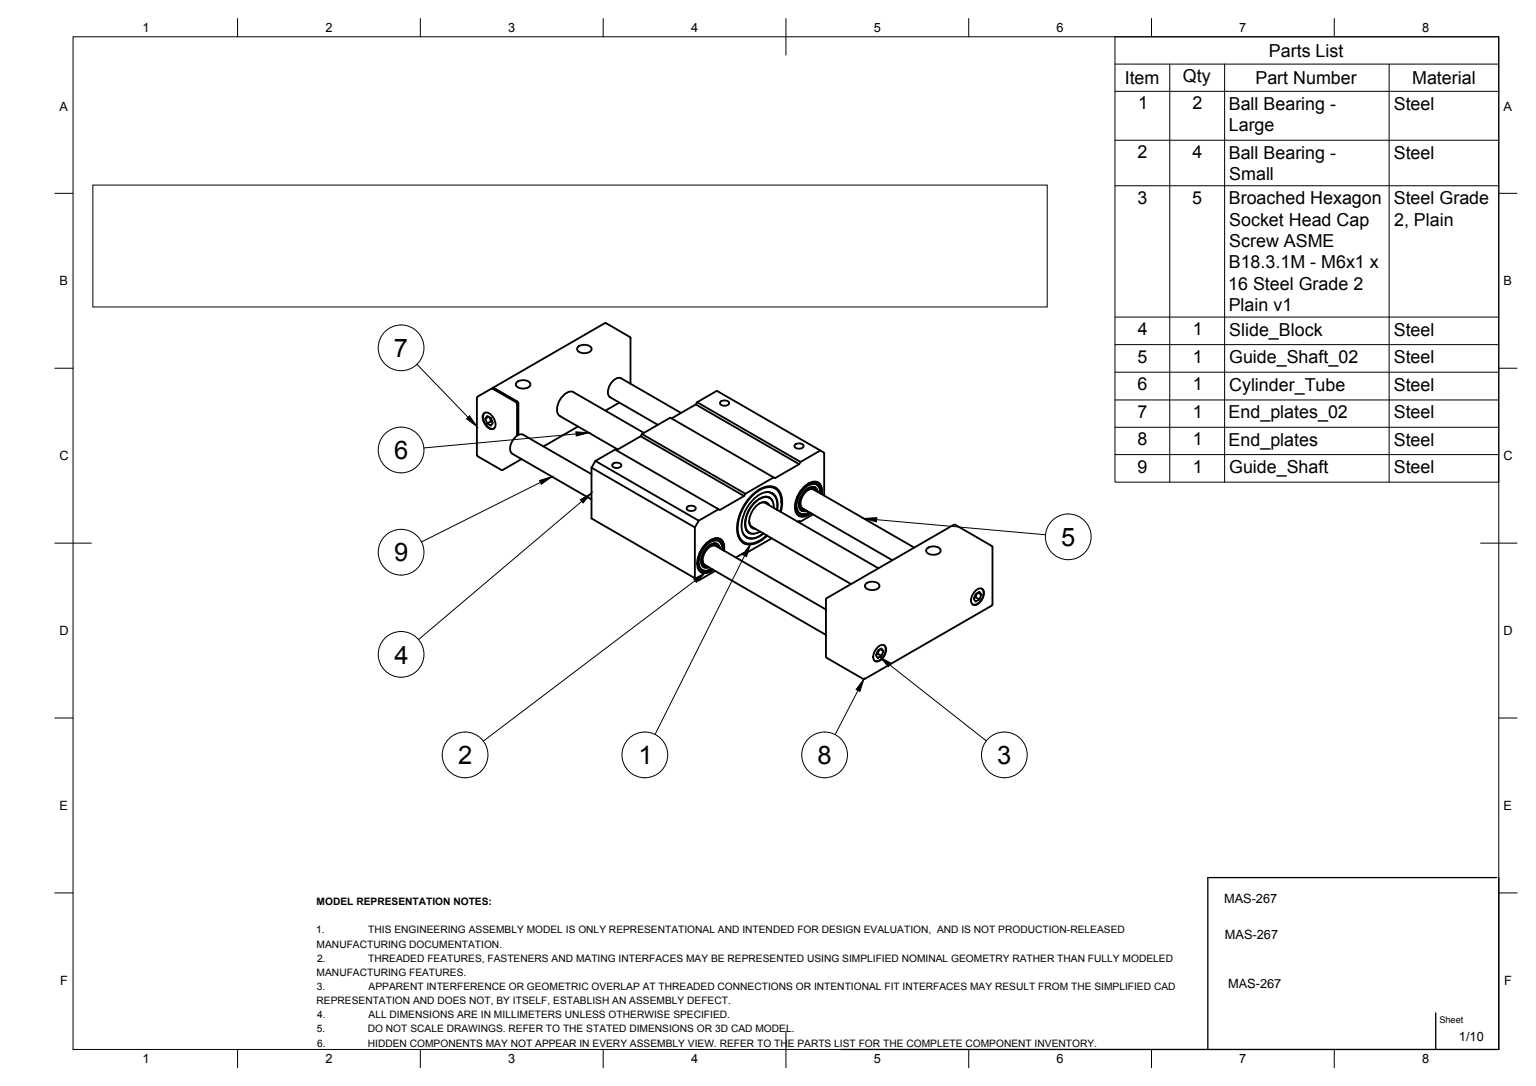
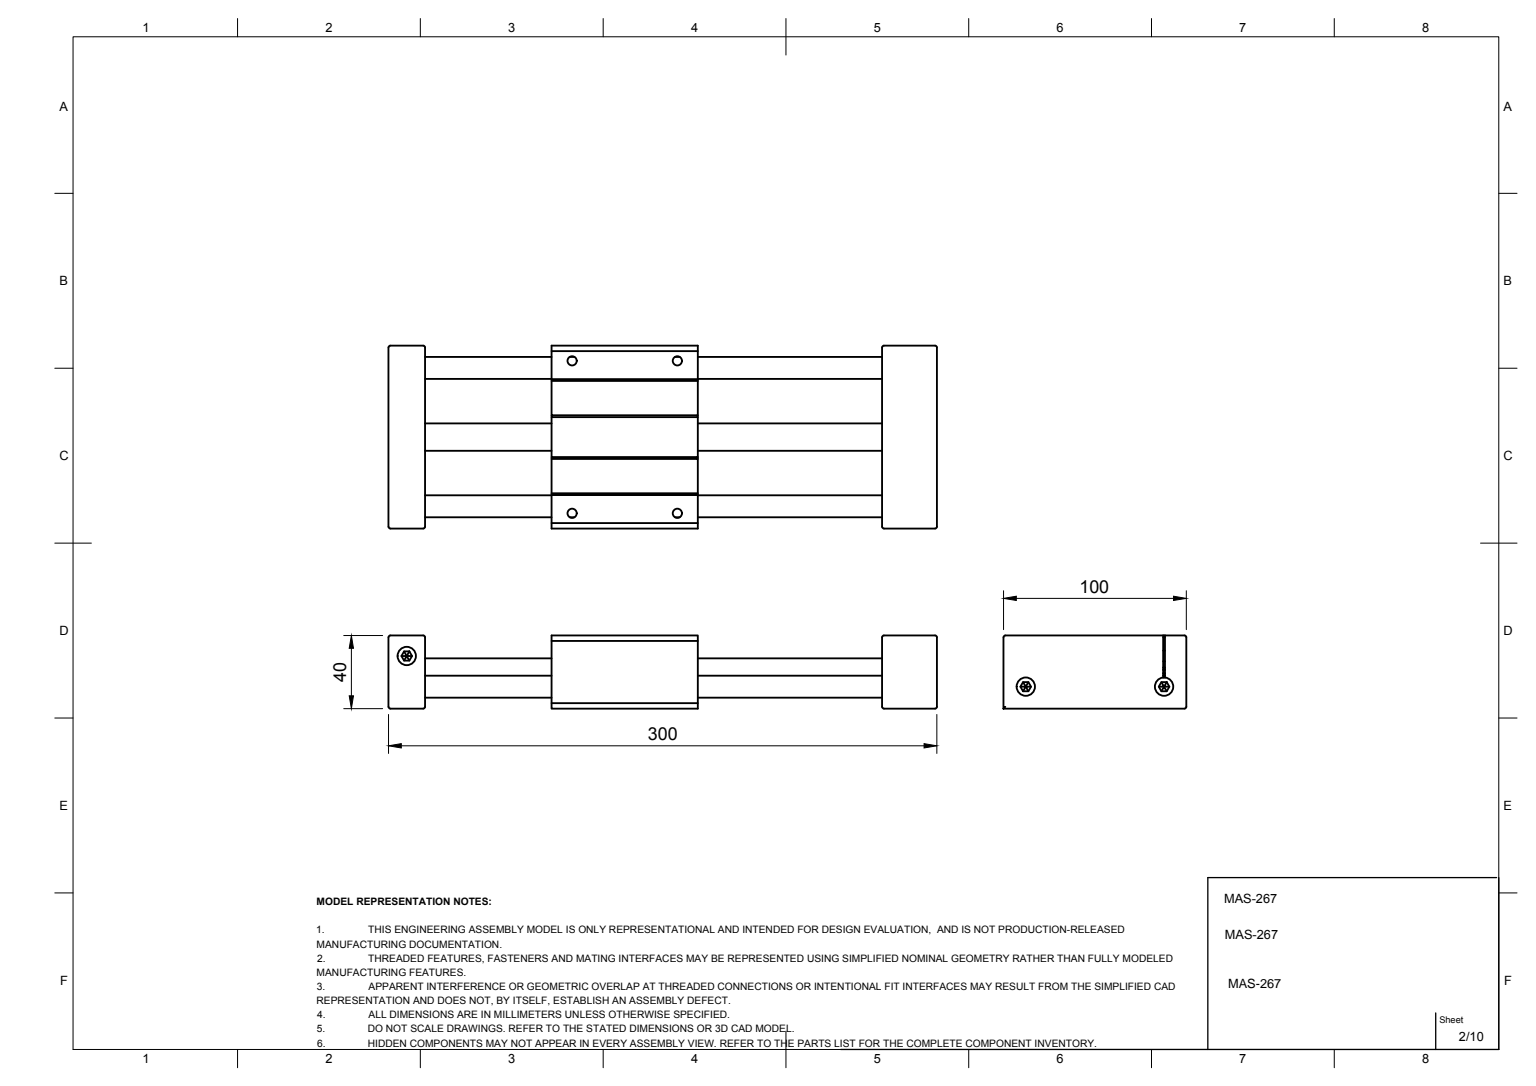
ISO-10303-21;
HEADER;
/* Generated by software containing ST-Developer
 * from STEP Tools, Inc. (www.steptools.com) 
 */

FILE_DESCRIPTION(
/* description */ (''),
/* implementation_level */ '2;1');

FILE_NAME(
/* name */ 'MAS-267',
/* time_stamp */ '2026-10-12T15:29:24-07:00',
/* author */ (''),
/* organization */ (''),
/* preprocessor_version */ 'ST-DEVELOPER v20.2',
/* originating_system */ 'Autodesk Translation Framework v15.15.0.0',
/* authorisation */ '');

FILE_SCHEMA (('AUTOMOTIVE_DESIGN { 1 0 10303 214 3 1 1 }'));
ENDSEC;

DATA;
#10=MECHANICAL_DESIGN_GEOMETRIC_PRESENTATION_REPRESENTATION('',(#163,#164,
#165,#166,#167,#168,#169,#170,#171,#172,#173,#174,#175,#176,#177,#178,#179,
#180,#181,#182,#183,#184,#185,#186,#187,#188,#189,#190,#191,#192,#193,#194,
#195,#196,#197,#198,#199,#200,#201,#202,#203,#204,#205,#206,#207,#208,#209,
#210,#211,#212,#213,#214,#215,#216,#217,#218,#219),#9496);
#11=ITEM_DEFINED_TRANSFORMATION($,$,#5298,#5809);
#12=ITEM_DEFINED_TRANSFORMATION($,$,#5515,#5810);
#13=ITEM_DEFINED_TRANSFORMATION($,$,#5515,#5811);
#14=ITEM_DEFINED_TRANSFORMATION($,$,#5123,#5812);
#15=ITEM_DEFINED_TRANSFORMATION($,$,#5213,#5813);
#16=ITEM_DEFINED_TRANSFORMATION($,$,#5298,#5814);
#17=ITEM_DEFINED_TRANSFORMATION($,$,#5298,#5815);
#18=ITEM_DEFINED_TRANSFORMATION($,$,#5298,#5816);
#19=ITEM_DEFINED_TRANSFORMATION($,$,#5515,#5817);
#20=ITEM_DEFINED_TRANSFORMATION($,$,#5515,#5818);
#21=ITEM_DEFINED_TRANSFORMATION($,$,#5515,#5819);
#22=ITEM_DEFINED_TRANSFORMATION($,$,#5542,#5820);
#23=ITEM_DEFINED_TRANSFORMATION($,$,#5556,#5821);
#24=ITEM_DEFINED_TRANSFORMATION($,$,#5562,#5822);
#25=ITEM_DEFINED_TRANSFORMATION($,$,#5576,#5823);
#26=ITEM_DEFINED_TRANSFORMATION($,$,#5576,#5824);
#27=ITEM_DEFINED_TRANSFORMATION($,$,#5757,#5825);
#28=(
REPRESENTATION_RELATIONSHIP($,$,#9541,#9538)
REPRESENTATION_RELATIONSHIP_WITH_TRANSFORMATION(#11)
SHAPE_REPRESENTATION_RELATIONSHIP()
);
#29=(
REPRESENTATION_RELATIONSHIP($,$,#9542,#9538)
REPRESENTATION_RELATIONSHIP_WITH_TRANSFORMATION(#12)
SHAPE_REPRESENTATION_RELATIONSHIP()
);
#30=(
REPRESENTATION_RELATIONSHIP($,$,#9542,#9538)
REPRESENTATION_RELATIONSHIP_WITH_TRANSFORMATION(#13)
SHAPE_REPRESENTATION_RELATIONSHIP()
);
#31=(
REPRESENTATION_RELATIONSHIP($,$,#9539,#9538)
REPRESENTATION_RELATIONSHIP_WITH_TRANSFORMATION(#14)
SHAPE_REPRESENTATION_RELATIONSHIP()
);
#32=(
REPRESENTATION_RELATIONSHIP($,$,#9540,#9538)
REPRESENTATION_RELATIONSHIP_WITH_TRANSFORMATION(#15)
SHAPE_REPRESENTATION_RELATIONSHIP()
);
#33=(
REPRESENTATION_RELATIONSHIP($,$,#9541,#9538)
REPRESENTATION_RELATIONSHIP_WITH_TRANSFORMATION(#16)
SHAPE_REPRESENTATION_RELATIONSHIP()
);
#34=(
REPRESENTATION_RELATIONSHIP($,$,#9541,#9538)
REPRESENTATION_RELATIONSHIP_WITH_TRANSFORMATION(#17)
SHAPE_REPRESENTATION_RELATIONSHIP()
);
#35=(
REPRESENTATION_RELATIONSHIP($,$,#9541,#9538)
REPRESENTATION_RELATIONSHIP_WITH_TRANSFORMATION(#18)
SHAPE_REPRESENTATION_RELATIONSHIP()
);
#36=(
REPRESENTATION_RELATIONSHIP($,$,#9542,#9538)
REPRESENTATION_RELATIONSHIP_WITH_TRANSFORMATION(#19)
SHAPE_REPRESENTATION_RELATIONSHIP()
);
#37=(
REPRESENTATION_RELATIONSHIP($,$,#9542,#9538)
REPRESENTATION_RELATIONSHIP_WITH_TRANSFORMATION(#20)
SHAPE_REPRESENTATION_RELATIONSHIP()
);
#38=(
REPRESENTATION_RELATIONSHIP($,$,#9542,#9538)
REPRESENTATION_RELATIONSHIP_WITH_TRANSFORMATION(#21)
SHAPE_REPRESENTATION_RELATIONSHIP()
);
#39=(
REPRESENTATION_RELATIONSHIP($,$,#9543,#9538)
REPRESENTATION_RELATIONSHIP_WITH_TRANSFORMATION(#22)
SHAPE_REPRESENTATION_RELATIONSHIP()
);
#40=(
REPRESENTATION_RELATIONSHIP($,$,#9544,#9538)
REPRESENTATION_RELATIONSHIP_WITH_TRANSFORMATION(#23)
SHAPE_REPRESENTATION_RELATIONSHIP()
);
#41=(
REPRESENTATION_RELATIONSHIP($,$,#9545,#9538)
REPRESENTATION_RELATIONSHIP_WITH_TRANSFORMATION(#24)
SHAPE_REPRESENTATION_RELATIONSHIP()
);
#42=(
REPRESENTATION_RELATIONSHIP($,$,#9546,#9538)
REPRESENTATION_RELATIONSHIP_WITH_TRANSFORMATION(#25)
SHAPE_REPRESENTATION_RELATIONSHIP()
);
#43=(
REPRESENTATION_RELATIONSHIP($,$,#9546,#9538)
REPRESENTATION_RELATIONSHIP_WITH_TRANSFORMATION(#26)
SHAPE_REPRESENTATION_RELATIONSHIP()
);
#44=(
REPRESENTATION_RELATIONSHIP($,$,#9547,#9538)
REPRESENTATION_RELATIONSHIP_WITH_TRANSFORMATION(#27)
SHAPE_REPRESENTATION_RELATIONSHIP()
);
#45=CONTEXT_DEPENDENT_SHAPE_REPRESENTATION(#28,#9521);
#46=CONTEXT_DEPENDENT_SHAPE_REPRESENTATION(#29,#9522);
#47=CONTEXT_DEPENDENT_SHAPE_REPRESENTATION(#30,#9523);
#48=CONTEXT_DEPENDENT_SHAPE_REPRESENTATION(#31,#9524);
#49=CONTEXT_DEPENDENT_SHAPE_REPRESENTATION(#32,#9525);
#50=CONTEXT_DEPENDENT_SHAPE_REPRESENTATION(#33,#9526);
#51=CONTEXT_DEPENDENT_SHAPE_REPRESENTATION(#34,#9527);
#52=CONTEXT_DEPENDENT_SHAPE_REPRESENTATION(#35,#9528);
#53=CONTEXT_DEPENDENT_SHAPE_REPRESENTATION(#36,#9529);
#54=CONTEXT_DEPENDENT_SHAPE_REPRESENTATION(#37,#9530);
#55=CONTEXT_DEPENDENT_SHAPE_REPRESENTATION(#38,#9531);
#56=CONTEXT_DEPENDENT_SHAPE_REPRESENTATION(#39,#9532);
#57=CONTEXT_DEPENDENT_SHAPE_REPRESENTATION(#40,#9533);
#58=CONTEXT_DEPENDENT_SHAPE_REPRESENTATION(#41,#9534);
#59=CONTEXT_DEPENDENT_SHAPE_REPRESENTATION(#42,#9535);
#60=CONTEXT_DEPENDENT_SHAPE_REPRESENTATION(#43,#9536);
#61=CONTEXT_DEPENDENT_SHAPE_REPRESENTATION(#44,#9537);
#62=NEXT_ASSEMBLY_USAGE_OCCURRENCE('Ball Bearing - Small:1',
'Ball Bearing - Small:1','Ball Bearing - Small:1',#9549,#9552,
'Ball Bearing - Small:1');
#63=NEXT_ASSEMBLY_USAGE_OCCURRENCE(
'Broached Hexagon Socket Head Cap Screw ASME B18.3.1M - M6x1 x 16 Stee
l Grade 2 Plain v1:1',
'Broached Hexagon Socket Head Cap Screw ASME B18.3.1M - M6x1 x 16 Stee
l Grade 2 Plain v1:1',
'Broached Hexagon Socket Head Cap Screw ASME B18.3.1M - M6x1 x 16 Stee
l Grade 2 Plain v1:1',#9549,#9553,
'Broached Hexagon Socket Head Cap Screw ASME B18.3.1M - M6x1 x 16 Stee
l Grade 2 Plain v1:1');
#64=NEXT_ASSEMBLY_USAGE_OCCURRENCE(
'Broached Hexagon Socket Head Cap Screw ASME B18.3.1M - M6x1 x 16 Stee
l Grade 2 Plain v1:2',
'Broached Hexagon Socket Head Cap Screw ASME B18.3.1M - M6x1 x 16 Stee
l Grade 2 Plain v1:2',
'Broached Hexagon Socket Head Cap Screw ASME B18.3.1M - M6x1 x 16 Stee
l Grade 2 Plain v1:2',#9549,#9553,
'Broached Hexagon Socket Head Cap Screw ASME B18.3.1M - M6x1 x 16 Stee
l Grade 2 Plain v1:2');
#65=NEXT_ASSEMBLY_USAGE_OCCURRENCE('End_plates_02:1','End_plates_02:1',
'End_plates_02:1',#9549,#9550,'End_plates_02:1');
#66=NEXT_ASSEMBLY_USAGE_OCCURRENCE('End_plates:1','End_plates:1',
'End_plates:1',#9549,#9551,'End_plates:1');
#67=NEXT_ASSEMBLY_USAGE_OCCURRENCE('Ball Bearing - Small:2',
'Ball Bearing - Small:2','Ball Bearing - Small:2',#9549,#9552,
'Ball Bearing - Small:2');
#68=NEXT_ASSEMBLY_USAGE_OCCURRENCE('Ball Bearing - Small:3',
'Ball Bearing - Small:3','Ball Bearing - Small:3',#9549,#9552,
'Ball Bearing - Small:3');
#69=NEXT_ASSEMBLY_USAGE_OCCURRENCE('Ball Bearing - Small:4',
'Ball Bearing - Small:4','Ball Bearing - Small:4',#9549,#9552,
'Ball Bearing - Small:4');
#70=NEXT_ASSEMBLY_USAGE_OCCURRENCE(
'Broached Hexagon Socket Head Cap Screw ASME B18.3.1M - M6x1 x 16 Stee
l Grade 2 Plain v1:3',
'Broached Hexagon Socket Head Cap Screw ASME B18.3.1M - M6x1 x 16 Stee
l Grade 2 Plain v1:3',
'Broached Hexagon Socket Head Cap Screw ASME B18.3.1M - M6x1 x 16 Stee
l Grade 2 Plain v1:3',#9549,#9553,
'Broached Hexagon Socket Head Cap Screw ASME B18.3.1M - M6x1 x 16 Stee
l Grade 2 Plain v1:3');
#71=NEXT_ASSEMBLY_USAGE_OCCURRENCE(
'Broached Hexagon Socket Head Cap Screw ASME B18.3.1M - M6x1 x 16 Stee
l Grade 2 Plain v1:4',
'Broached Hexagon Socket Head Cap Screw ASME B18.3.1M - M6x1 x 16 Stee
l Grade 2 Plain v1:4',
'Broached Hexagon Socket Head Cap Screw ASME B18.3.1M - M6x1 x 16 Stee
l Grade 2 Plain v1:4',#9549,#9553,
'Broached Hexagon Socket Head Cap Screw ASME B18.3.1M - M6x1 x 16 Stee
l Grade 2 Plain v1:4');
#72=NEXT_ASSEMBLY_USAGE_OCCURRENCE(
'Broached Hexagon Socket Head Cap Screw ASME B18.3.1M - M6x1 x 16 Stee
l Grade 2 Plain v1:5',
'Broached Hexagon Socket Head Cap Screw ASME B18.3.1M - M6x1 x 16 Stee
l Grade 2 Plain v1:5',
'Broached Hexagon Socket Head Cap Screw ASME B18.3.1M - M6x1 x 16 Stee
l Grade 2 Plain v1:5',#9549,#9553,
'Broached Hexagon Socket Head Cap Screw ASME B18.3.1M - M6x1 x 16 Stee
l Grade 2 Plain v1:5');
#73=NEXT_ASSEMBLY_USAGE_OCCURRENCE('Guide_Shaft_02:1',
'Guide_Shaft_02:1','Guide_Shaft_02:1',#9549,#9554,'Guide_Shaft_02:1');
#74=NEXT_ASSEMBLY_USAGE_OCCURRENCE('Cylinder_Tube:1','Cylinder_Tube:1',
'Cylinder_Tube:1',#9549,#9555,'Cylinder_Tube:1');
#75=NEXT_ASSEMBLY_USAGE_OCCURRENCE('Guide_Shaft:1','Guide_Shaft:1',
'Guide_Shaft:1',#9549,#9556,'Guide_Shaft:1');
#76=NEXT_ASSEMBLY_USAGE_OCCURRENCE('Ball Bearing - Large:1',
'Ball Bearing - Large:1','Ball Bearing - Large:1',#9549,#9557,
'Ball Bearing - Large:1');
#77=NEXT_ASSEMBLY_USAGE_OCCURRENCE('Ball Bearing - Large:2',
'Ball Bearing - Large:2','Ball Bearing - Large:2',#9549,#9557,
'Ball Bearing - Large:2');
#78=NEXT_ASSEMBLY_USAGE_OCCURRENCE('Slide_Block:1','Slide_Block:1',
'Slide_Block:1',#9549,#9558,'Slide_Block:1');
#79=B_SPLINE_CURVE_WITH_KNOTS('',3,(#8964,#8965,#8966,#8967,#8968,#8969,
#8970,#8971,#8972,#8973),.UNSPECIFIED.,.F.,.F.,(4,2,2,2,4),(-1.57648415340294,
-1.48130138260372,-1.38611861180451,-1.27940954804234,-1.17270048428017),
 .UNSPECIFIED.);
#80=B_SPLINE_CURVE_WITH_KNOTS('',3,(#8974,#8975,#8976,#8977,#8978,#8979,
#8980,#8981,#8982,#8983,#8984,#8985,#8986,#8987,#8988,#8989,#8990,#8991,
#8992,#8993,#8994,#8995,#8996,#8997,#8998,#8999),.UNSPECIFIED.,.F.,.F.,
(4,2,2,2,2,2,2,2,2,2,2,2,4),(-1.17270048428017,-1.07435447096729,-0.976008457654416,
-0.882125267177943,-0.78824207670147,-0.694358886224997,-0.600475695748524,
-0.502129682435648,-0.403783669122773,-0.297074605360601,-0.190365541598429,
-0.0951827707992146,0.),.UNSPECIFIED.);
#81=B_SPLINE_CURVE_WITH_KNOTS('',3,(#9003,#9004,#9005,#9006,#9007,#9008,
#9009,#9010,#9011,#9012,#9013,#9014,#9015,#9016,#9017,#9018,#9019,#9020,
#9021,#9022,#9023,#9024,#9025,#9026,#9027,#9028),.UNSPECIFIED.,.F.,.F.,
(4,2,2,2,2,2,2,2,2,2,2,2,4),(-1.57648415340294,-1.48130138260372,-1.38611861180451,
-1.27940954804234,-1.17270048428017,-1.07435447096729,-0.976008457654416,
-0.882125267177943,-0.78824207670147,-0.694358886224997,-0.600475695748524,
-0.502129682435648,-0.403783669122773),.UNSPECIFIED.);
#82=B_SPLINE_CURVE_WITH_KNOTS('',3,(#9029,#9030,#9031,#9032,#9033,#9034,
#9035,#9036,#9037,#9038),.UNSPECIFIED.,.F.,.F.,(4,2,2,2,4),(-0.403783669122773,
-0.297074605360601,-0.190365541598429,-0.0951827707992147,0.),
 .UNSPECIFIED.);
#83=B_SPLINE_CURVE_WITH_KNOTS('',3,(#9048,#9049,#9050,#9051,#9052,#9053,
#9054,#9055,#9056,#9057,#9058,#9059,#9060,#9061,#9062,#9063,#9064,#9065,
#9066,#9067,#9068,#9069,#9070,#9071,#9072,#9073),.UNSPECIFIED.,.F.,.F.,
(4,2,2,2,2,2,2,2,2,2,2,2,4),(-1.57648415340294,-1.48130138260372,-1.38611861180451,
-1.27940954804234,-1.17270048428017,-1.07435447096729,-0.976008457654416,
-0.882125267177943,-0.78824207670147,-0.694358886224997,-0.600475695748524,
-0.502129682435648,-0.403783669122773),.UNSPECIFIED.);
#84=B_SPLINE_CURVE_WITH_KNOTS('',3,(#9074,#9075,#9076,#9077,#9078,#9079,
#9080,#9081,#9082,#9083),.UNSPECIFIED.,.F.,.F.,(4,2,2,2,4),(-0.403783669122773,
-0.297074605360601,-0.190365541598429,-0.0951827707992146,0.),
 .UNSPECIFIED.);
#85=B_SPLINE_CURVE_WITH_KNOTS('',3,(#9087,#9088,#9089,#9090,#9091,#9092,
#9093,#9094,#9095,#9096),.UNSPECIFIED.,.F.,.F.,(4,2,2,2,4),(-1.57648415340294,
-1.48130138260372,-1.38611861180451,-1.27940954804234,-1.17270048428017),
 .UNSPECIFIED.);
#86=B_SPLINE_CURVE_WITH_KNOTS('',3,(#9097,#9098,#9099,#9100,#9101,#9102,
#9103,#9104,#9105,#9106,#9107,#9108,#9109,#9110,#9111,#9112,#9113,#9114,
#9115,#9116,#9117,#9118,#9119,#9120,#9121,#9122),.UNSPECIFIED.,.F.,.F.,
(4,2,2,2,2,2,2,2,2,2,2,2,4),(-1.17270048428017,-1.07435447096729,-0.976008457654416,
-0.882125267177943,-0.78824207670147,-0.694358886224997,-0.600475695748524,
-0.502129682435648,-0.403783669122773,-0.297074605360601,-0.190365541598429,
-0.0951827707992147,0.),.UNSPECIFIED.);
#87=B_SPLINE_CURVE_WITH_KNOTS('',3,(#9132,#9133,#9134,#9135,#9136,#9137,
#9138,#9139,#9140,#9141),.UNSPECIFIED.,.F.,.F.,(4,2,2,2,4),(-1.57648415340294,
-1.48130138260372,-1.38611861180451,-1.27940954804234,-1.17270048428017),
 .UNSPECIFIED.);
#88=B_SPLINE_CURVE_WITH_KNOTS('',3,(#9142,#9143,#9144,#9145,#9146,#9147,
#9148,#9149,#9150,#9151,#9152,#9153,#9154,#9155,#9156,#9157,#9158,#9159,
#9160,#9161,#9162,#9163,#9164,#9165,#9166,#9167),.UNSPECIFIED.,.F.,.F.,
(4,2,2,2,2,2,2,2,2,2,2,2,4),(-1.17270048428017,-1.07435447096729,-0.976008457654416,
-0.882125267177943,-0.78824207670147,-0.694358886224997,-0.600475695748524,
-0.502129682435648,-0.403783669122773,-0.297074605360601,-0.190365541598429,
-0.0951827707992146,0.),.UNSPECIFIED.);
#89=B_SPLINE_CURVE_WITH_KNOTS('',3,(#9171,#9172,#9173,#9174,#9175,#9176,
#9177,#9178,#9179,#9180,#9181,#9182,#9183,#9184,#9185,#9186,#9187,#9188,
#9189,#9190,#9191,#9192,#9193,#9194,#9195,#9196),.UNSPECIFIED.,.F.,.F.,
(4,2,2,2,2,2,2,2,2,2,2,2,4),(-1.57648415340294,-1.48130138260372,-1.38611861180451,
-1.27940954804234,-1.17270048428017,-1.07435447096729,-0.976008457654416,
-0.882125267177943,-0.78824207670147,-0.694358886224997,-0.600475695748524,
-0.502129682435648,-0.403783669122773),.UNSPECIFIED.);
#90=B_SPLINE_CURVE_WITH_KNOTS('',3,(#9197,#9198,#9199,#9200,#9201,#9202,
#9203,#9204,#9205,#9206),.UNSPECIFIED.,.F.,.F.,(4,2,2,2,4),(-0.403783669122773,
-0.297074605360601,-0.190365541598429,-0.0951827707992147,0.),
 .UNSPECIFIED.);
#91=B_SPLINE_CURVE_WITH_KNOTS('',3,(#9216,#9217,#9218,#9219,#9220,#9221,
#9222,#9223,#9224,#9225,#9226,#9227,#9228,#9229,#9230,#9231,#9232,#9233,
#9234,#9235,#9236,#9237,#9238,#9239,#9240,#9241),.UNSPECIFIED.,.F.,.F.,
(4,2,2,2,2,2,2,2,2,2,2,2,4),(-1.57648415340294,-1.48130138260372,-1.38611861180451,
-1.27940954804234,-1.17270048428017,-1.07435447096729,-0.976008457654416,
-0.882125267177943,-0.78824207670147,-0.694358886224997,-0.600475695748524,
-0.502129682435648,-0.403783669122773),.UNSPECIFIED.);
#92=B_SPLINE_CURVE_WITH_KNOTS('',3,(#9242,#9243,#9244,#9245,#9246,#9247,
#9248,#9249,#9250,#9251),.UNSPECIFIED.,.F.,.F.,(4,2,2,2,4),(-0.403783669122773,
-0.297074605360601,-0.190365541598429,-0.0951827707992146,0.),
 .UNSPECIFIED.);
#93=B_SPLINE_CURVE_WITH_KNOTS('',3,(#9255,#9256,#9257,#9258,#9259,#9260,
#9261,#9262,#9263,#9264),.UNSPECIFIED.,.F.,.F.,(4,2,2,2,4),(-1.57648415340294,
-1.48130138260372,-1.38611861180451,-1.27940954804234,-1.17270048428017),
 .UNSPECIFIED.);
#94=B_SPLINE_CURVE_WITH_KNOTS('',3,(#9265,#9266,#9267,#9268,#9269,#9270,
#9271,#9272,#9273,#9274,#9275,#9276,#9277,#9278,#9279,#9280,#9281,#9282,
#9283,#9284,#9285,#9286,#9287,#9288,#9289,#9290),.UNSPECIFIED.,.F.,.F.,
(4,2,2,2,2,2,2,2,2,2,2,2,4),(-1.17270048428017,-1.07435447096729,-0.976008457654416,
-0.882125267177943,-0.78824207670147,-0.694358886224997,-0.600475695748524,
-0.502129682435648,-0.403783669122773,-0.297074605360601,-0.190365541598429,
-0.0951827707992147,0.),.UNSPECIFIED.);
#95=(
BOUNDED_SURFACE()
B_SPLINE_SURFACE(2,2,((#7928,#7929,#7930,#7931,#7932,#7933,#7934,#7935,
#7936),(#7937,#7938,#7939,#7940,#7941,#7942,#7943,#7944,#7945),(#7946,#7947,
#7948,#7949,#7950,#7951,#7952,#7953,#7954)),.UNSPECIFIED.,.F.,.T.,.F.)
B_SPLINE_SURFACE_WITH_KNOTS((3,3),(3,2,2,2,3),(-0.359817990374321,0.359817990374321),
(-3.14159265358979,-1.5707963267949,0.,1.5707963267949,3.14159265358979),
 .UNSPECIFIED.)
GEOMETRIC_REPRESENTATION_ITEM()
RATIONAL_B_SPLINE_SURFACE(((1.,0.707106781186548,1.,0.707106781186548,1.,
0.707106781186548,1.,0.707106781186548,1.),(0.935960925476955,0.661824317330392,
0.935960925476955,0.661824317330392,0.935960925476955,0.661824317330392,
0.935960925476955,0.661824317330392,0.935960925476955),(1.,0.707106781186548,
1.,0.707106781186548,1.,0.707106781186548,1.,0.707106781186548,1.)))
REPRESENTATION_ITEM('')
SURFACE()
);
#96=(
BOUNDED_SURFACE()
B_SPLINE_SURFACE(2,2,((#7970,#7971,#7972,#7973,#7974,#7975,#7976,#7977,
#7978),(#7979,#7980,#7981,#7982,#7983,#7984,#7985,#7986,#7987),(#7988,#7989,
#7990,#7991,#7992,#7993,#7994,#7995,#7996)),.UNSPECIFIED.,.F.,.T.,.F.)
B_SPLINE_SURFACE_WITH_KNOTS((3,3),(3,2,2,2,3),(-0.359817990374415,0.359817990374426),
(-3.14159265358979,-1.5707963267949,0.,1.5707963267949,3.14159265358979),
 .UNSPECIFIED.)
GEOMETRIC_REPRESENTATION_ITEM()
RATIONAL_B_SPLINE_SURFACE(((1.,0.707106781186548,1.,0.707106781186548,1.,
0.707106781186548,1.,0.707106781186548,1.),(0.935960925476919,0.661824317330366,
0.935960925476919,0.661824317330366,0.935960925476919,0.661824317330366,
0.935960925476919,0.661824317330366,0.935960925476919),(1.,0.707106781186548,
1.,0.707106781186548,1.,0.707106781186548,1.,0.707106781186548,1.)))
REPRESENTATION_ITEM('')
SURFACE()
);
#97=(
BOUNDED_SURFACE()
B_SPLINE_SURFACE(2,2,((#8012,#8013,#8014,#8015,#8016,#8017,#8018,#8019,
#8020),(#8021,#8022,#8023,#8024,#8025,#8026,#8027,#8028,#8029),(#8030,#8031,
#8032,#8033,#8034,#8035,#8036,#8037,#8038)),.UNSPECIFIED.,.F.,.T.,.F.)
B_SPLINE_SURFACE_WITH_KNOTS((3,3),(3,2,2,2,3),(-0.359817990374342,0.359817990374333),
(-3.14159265358979,-1.5707963267949,0.,1.5707963267949,3.14159265358979),
 .UNSPECIFIED.)
GEOMETRIC_REPRESENTATION_ITEM()
RATIONAL_B_SPLINE_SURFACE(((1.,0.707106781186548,1.,0.707106781186548,1.,
0.707106781186548,1.,0.707106781186548,1.),(0.935960925476941,0.661824317330382,
0.935960925476941,0.661824317330382,0.935960925476941,0.661824317330382,
0.935960925476941,0.661824317330382,0.935960925476941),(1.,0.707106781186548,
1.,0.707106781186548,1.,0.707106781186548,1.,0.707106781186548,1.)))
REPRESENTATION_ITEM('')
SURFACE()
);
#98=(
BOUNDED_SURFACE()
B_SPLINE_SURFACE(2,2,((#8054,#8055,#8056,#8057,#8058,#8059,#8060,#8061,
#8062),(#8063,#8064,#8065,#8066,#8067,#8068,#8069,#8070,#8071),(#8072,#8073,
#8074,#8075,#8076,#8077,#8078,#8079,#8080)),.UNSPECIFIED.,.F.,.T.,.F.)
B_SPLINE_SURFACE_WITH_KNOTS((3,3),(3,2,2,2,3),(-0.359817990374327,0.359817990374343),
(-3.14159265358979,-1.5707963267949,0.,1.5707963267949,3.14159265358979),
 .UNSPECIFIED.)
GEOMETRIC_REPRESENTATION_ITEM()
RATIONAL_B_SPLINE_SURFACE(((1.,0.707106781186548,1.,0.707106781186548,1.,
0.707106781186548,1.,0.707106781186548,1.),(0.935960925476945,0.661824317330385,
0.935960925476945,0.661824317330385,0.935960925476945,0.661824317330385,
0.935960925476945,0.661824317330385,0.935960925476945),(1.,0.707106781186548,
1.,0.707106781186548,1.,0.707106781186548,1.,0.707106781186548,1.)))
REPRESENTATION_ITEM('')
SURFACE()
);
#99=(
BOUNDED_SURFACE()
B_SPLINE_SURFACE(2,2,((#8096,#8097,#8098,#8099,#8100,#8101,#8102,#8103,
#8104),(#8105,#8106,#8107,#8108,#8109,#8110,#8111,#8112,#8113),(#8114,#8115,
#8116,#8117,#8118,#8119,#8120,#8121,#8122)),.UNSPECIFIED.,.F.,.T.,.F.)
B_SPLINE_SURFACE_WITH_KNOTS((3,3),(3,2,2,2,3),(-0.359817990374369,0.359817990374379),
(-3.14159265358979,-1.5707963267949,0.,1.5707963267949,3.14159265358979),
 .UNSPECIFIED.)
GEOMETRIC_REPRESENTATION_ITEM()
RATIONAL_B_SPLINE_SURFACE(((1.,0.707106781186548,1.,0.707106781186548,1.,
0.707106781186548,1.,0.707106781186548,1.),(0.935960925476939,0.661824317330381,
0.935960925476939,0.661824317330381,0.935960925476939,0.661824317330381,
0.935960925476939,0.661824317330381,0.935960925476939),(1.,0.707106781186548,
1.,0.707106781186548,1.,0.707106781186548,1.,0.707106781186548,1.)))
REPRESENTATION_ITEM('')
SURFACE()
);
#100=(
BOUNDED_SURFACE()
B_SPLINE_SURFACE(2,2,((#8138,#8139,#8140,#8141,#8142,#8143,#8144,#8145,
#8146),(#8147,#8148,#8149,#8150,#8151,#8152,#8153,#8154,#8155),(#8156,#8157,
#8158,#8159,#8160,#8161,#8162,#8163,#8164)),.UNSPECIFIED.,.F.,.T.,.F.)
B_SPLINE_SURFACE_WITH_KNOTS((3,3),(3,2,2,2,3),(-0.359817990374391,0.359817990374391),
(-3.14159265358979,-1.5707963267949,0.,1.5707963267949,3.14159265358979),
 .UNSPECIFIED.)
GEOMETRIC_REPRESENTATION_ITEM()
RATIONAL_B_SPLINE_SURFACE(((1.,0.707106781186548,1.,0.707106781186548,1.,
0.707106781186548,1.,0.707106781186548,1.),(0.935960925476929,0.661824317330373,
0.935960925476929,0.661824317330373,0.935960925476929,0.661824317330373,
0.935960925476929,0.661824317330373,0.935960925476929),(1.,0.707106781186548,
1.,0.707106781186548,1.,0.707106781186548,1.,0.707106781186548,1.)))
REPRESENTATION_ITEM('')
SURFACE()
);
#101=(
BOUNDED_SURFACE()
B_SPLINE_SURFACE(2,2,((#8180,#8181,#8182,#8183,#8184,#8185,#8186,#8187,
#8188),(#8189,#8190,#8191,#8192,#8193,#8194,#8195,#8196,#8197),(#8198,#8199,
#8200,#8201,#8202,#8203,#8204,#8205,#8206)),.UNSPECIFIED.,.F.,.T.,.F.)
B_SPLINE_SURFACE_WITH_KNOTS((3,3),(3,2,2,2,3),(-0.359817990374328,0.359817990374325),
(-3.14159265358979,-1.5707963267949,0.,1.5707963267949,3.14159265358979),
 .UNSPECIFIED.)
GEOMETRIC_REPRESENTATION_ITEM()
RATIONAL_B_SPLINE_SURFACE(((1.,0.707106781186548,1.,0.707106781186548,1.,
0.707106781186548,1.,0.707106781186548,1.),(0.935960925476951,0.661824317330389,
0.935960925476951,0.661824317330389,0.935960925476951,0.661824317330389,
0.935960925476951,0.661824317330389,0.935960925476951),(1.,0.707106781186548,
1.,0.707106781186548,1.,0.707106781186548,1.,0.707106781186548,1.)))
REPRESENTATION_ITEM('')
SURFACE()
);
#102=(
BOUNDED_SURFACE()
B_SPLINE_SURFACE(2,2,((#8222,#8223,#8224,#8225,#8226,#8227,#8228,#8229,
#8230),(#8231,#8232,#8233,#8234,#8235,#8236,#8237,#8238,#8239),(#8240,#8241,
#8242,#8243,#8244,#8245,#8246,#8247,#8248)),.UNSPECIFIED.,.F.,.T.,.F.)
B_SPLINE_SURFACE_WITH_KNOTS((3,3),(3,2,2,2,3),(-0.359817990374346,0.359817990374343),
(-3.14159265358979,-1.5707963267949,0.,1.5707963267949,3.14159265358979),
 .UNSPECIFIED.)
GEOMETRIC_REPRESENTATION_ITEM()
RATIONAL_B_SPLINE_SURFACE(((1.,0.707106781186548,1.,0.707106781186548,1.,
0.707106781186548,1.,0.707106781186548,1.),(0.935960925476942,0.661824317330383,
0.935960925476942,0.661824317330383,0.935960925476942,0.661824317330383,
0.935960925476942,0.661824317330383,0.935960925476942),(1.,0.707106781186548,
1.,0.707106781186548,1.,0.707106781186548,1.,0.707106781186548,1.)))
REPRESENTATION_ITEM('')
SURFACE()
);
#103=(
BOUNDED_SURFACE()
B_SPLINE_SURFACE(2,2,((#8264,#8265,#8266,#8267,#8268,#8269,#8270,#8271,
#8272),(#8273,#8274,#8275,#8276,#8277,#8278,#8279,#8280,#8281),(#8282,#8283,
#8284,#8285,#8286,#8287,#8288,#8289,#8290)),.UNSPECIFIED.,.F.,.T.,.F.)
B_SPLINE_SURFACE_WITH_KNOTS((3,3),(3,2,2,2,3),(-0.359817990374353,0.359817990374347),
(-3.14159265358979,-1.5707963267949,0.,1.5707963267949,3.14159265358979),
 .UNSPECIFIED.)
GEOMETRIC_REPRESENTATION_ITEM()
RATIONAL_B_SPLINE_SURFACE(((1.,0.707106781186548,1.,0.707106781186548,1.,
0.707106781186548,1.,0.707106781186548,1.),(0.935960925476944,0.661824317330384,
0.935960925476944,0.661824317330384,0.935960925476944,0.661824317330384,
0.935960925476944,0.661824317330384,0.935960925476944),(1.,0.707106781186548,
1.,0.707106781186548,1.,0.707106781186548,1.,0.707106781186548,1.)))
REPRESENTATION_ITEM('')
SURFACE()
);
#104=(
BOUNDED_SURFACE()
B_SPLINE_SURFACE(2,2,((#8306,#8307,#8308,#8309,#8310,#8311,#8312,#8313,
#8314),(#8315,#8316,#8317,#8318,#8319,#8320,#8321,#8322,#8323),(#8324,#8325,
#8326,#8327,#8328,#8329,#8330,#8331,#8332)),.UNSPECIFIED.,.F.,.T.,.F.)
B_SPLINE_SURFACE_WITH_KNOTS((3,3),(3,2,2,2,3),(-0.359817990374389,0.359817990374389),
(-3.14159265358979,-1.5707963267949,0.,1.5707963267949,3.14159265358979),
 .UNSPECIFIED.)
GEOMETRIC_REPRESENTATION_ITEM()
RATIONAL_B_SPLINE_SURFACE(((1.,0.707106781186548,1.,0.707106781186548,1.,
0.707106781186548,1.,0.707106781186548,1.),(0.935960925476925,0.661824317330371,
0.935960925476925,0.661824317330371,0.935960925476925,0.661824317330371,
0.935960925476925,0.661824317330371,0.935960925476925),(1.,0.707106781186548,
1.,0.707106781186548,1.,0.707106781186548,1.,0.707106781186548,1.)))
REPRESENTATION_ITEM('')
SURFACE()
);
#105=(
BOUNDED_SURFACE()
B_SPLINE_SURFACE(2,2,((#8362,#8363,#8364,#8365,#8366,#8367,#8368,#8369,
#8370),(#8371,#8372,#8373,#8374,#8375,#8376,#8377,#8378,#8379),(#8380,#8381,
#8382,#8383,#8384,#8385,#8386,#8387,#8388)),.UNSPECIFIED.,.F.,.T.,.F.)
B_SPLINE_SURFACE_WITH_KNOTS((3,3),(3,2,2,2,3),(-0.359817990374337,0.359817990374338),
(-3.14159265358979,-1.5707963267949,0.,1.5707963267949,3.14159265358979),
 .UNSPECIFIED.)
GEOMETRIC_REPRESENTATION_ITEM()
RATIONAL_B_SPLINE_SURFACE(((1.,0.707106781186548,1.,0.707106781186548,1.,
0.707106781186548,1.,0.707106781186548,1.),(0.935960925476947,0.661824317330386,
0.935960925476947,0.661824317330386,0.935960925476947,0.661824317330386,
0.935960925476947,0.661824317330386,0.935960925476947),(1.,0.707106781186548,
1.,0.707106781186548,1.,0.707106781186548,1.,0.707106781186548,1.)))
REPRESENTATION_ITEM('')
SURFACE()
);
#106=(
BOUNDED_SURFACE()
B_SPLINE_SURFACE(2,2,((#8404,#8405,#8406,#8407,#8408,#8409,#8410,#8411,
#8412),(#8413,#8414,#8415,#8416,#8417,#8418,#8419,#8420,#8421),(#8422,#8423,
#8424,#8425,#8426,#8427,#8428,#8429,#8430)),.UNSPECIFIED.,.F.,.T.,.F.)
B_SPLINE_SURFACE_WITH_KNOTS((3,3),(3,2,2,2,3),(-0.359817990374313,0.359817990374317),
(-3.14159265358979,-1.5707963267949,0.,1.5707963267949,3.14159265358979),
 .UNSPECIFIED.)
GEOMETRIC_REPRESENTATION_ITEM()
RATIONAL_B_SPLINE_SURFACE(((1.,0.707106781186548,1.,0.707106781186548,1.,
0.707106781186548,1.,0.707106781186548,1.),(0.935960925476952,0.66182431733039,
0.935960925476952,0.66182431733039,0.935960925476952,0.66182431733039,0.935960925476952,
0.66182431733039,0.935960925476952),(1.,0.707106781186548,1.,0.707106781186548,
1.,0.707106781186548,1.,0.707106781186548,1.)))
REPRESENTATION_ITEM('')
SURFACE()
);
#107=CONICAL_SURFACE('',#5303,6.24999999999999,0.785398163397428);
#108=CONICAL_SURFACE('',#5309,6.,0.785398163397428);
#109=CONICAL_SURFACE('',#5319,10.25,0.785398163397433);
#110=CONICAL_SURFACE('',#5330,10.5,0.785398163397433);
#111=CONICAL_SURFACE('',#5488,9.25000000000001,1.01776488264426);
#112=CONICAL_SURFACE('',#5490,7.39999999999999,1.01776488264426);
#113=CONICAL_SURFACE('',#5507,7.24999999999999,1.01776488264426);
#114=CONICAL_SURFACE('',#5509,9.1,1.01776488264426);
#115=CONICAL_SURFACE('',#5516,2.72327499999996,0.831988093682975);
#116=CONICAL_SURFACE('',#5581,8.04999999999999,0.78539816339744);
#117=CONICAL_SURFACE('',#5587,7.5,0.78539816339744);
#118=CONICAL_SURFACE('',#5597,16.95,0.785398163397447);
#119=CONICAL_SURFACE('',#5608,17.5,0.785398163397446);
#120=CONICAL_SURFACE('',#5730,14.,0.835033387742089);
#121=CONICAL_SURFACE('',#5732,11.225,0.835033387742081);
#122=CONICAL_SURFACE('',#5749,11.,0.835033387742083);
#123=CONICAL_SURFACE('',#5751,13.775,0.835033387742092);
#124=TOROIDAL_SURFACE('',#5299,8.25,1.49484711634153);
#125=TOROIDAL_SURFACE('',#5325,8.25,1.49484711634153);
#126=TOROIDAL_SURFACE('',#5475,7.42777777777777,0.0277777777777778);
#127=TOROIDAL_SURFACE('',#5480,9.07222222222223,0.0277777777777778);
#128=TOROIDAL_SURFACE('',#5496,9.07222222222222,0.027777777777778);
#129=TOROIDAL_SURFACE('',#5500,7.42777777777777,0.027777777777778);
#130=TOROIDAL_SURFACE('',#5519,4.39999999999977,0.6);
#131=TOROIDAL_SURFACE('',#5577,12.5,2.86797988869785);
#132=TOROIDAL_SURFACE('',#5603,12.5,2.86797988869785);
#133=TOROIDAL_SURFACE('',#5629,2.10186832938358,1.34926506255229);
#134=TOROIDAL_SURFACE('',#5639,2.10186832938358,1.34926506255229);
#135=TOROIDAL_SURFACE('',#5649,2.10186832938358,1.34926506255229);
#136=TOROIDAL_SURFACE('',#5659,2.10186832938358,1.34926506255229);
#137=TOROIDAL_SURFACE('',#5669,2.10186832938358,1.34926506255229);
#138=TOROIDAL_SURFACE('',#5679,2.10186832938358,1.34926506255229);
#139=TOROIDAL_SURFACE('',#5689,2.10186832938358,1.34926506255229);
#140=TOROIDAL_SURFACE('',#5699,2.10186832938358,1.34926506255229);
#141=TOROIDAL_SURFACE('',#5717,11.2861111111111,0.0611111111111111);
#142=TOROIDAL_SURFACE('',#5722,13.7138888888889,0.0611111111111111);
#143=TOROIDAL_SURFACE('',#5738,13.7138888888889,0.061111111111111);
#144=TOROIDAL_SURFACE('',#5742,11.2861111111111,0.061111111111111);
#145=SHAPE_REPRESENTATION_RELATIONSHIP('SRR','None',#9539,#154);
#146=SHAPE_REPRESENTATION_RELATIONSHIP('SRR','None',#9540,#155);
#147=SHAPE_REPRESENTATION_RELATIONSHIP('SRR','None',#9541,#156);
#148=SHAPE_REPRESENTATION_RELATIONSHIP('SRR','None',#9542,#157);
#149=SHAPE_REPRESENTATION_RELATIONSHIP('SRR','None',#9543,#158);
#150=SHAPE_REPRESENTATION_RELATIONSHIP('SRR','None',#9544,#159);
#151=SHAPE_REPRESENTATION_RELATIONSHIP('SRR','None',#9545,#160);
#152=SHAPE_REPRESENTATION_RELATIONSHIP('SRR','None',#9546,#161);
#153=SHAPE_REPRESENTATION_RELATIONSHIP('SRR','None',#9547,#162);
#154=ADVANCED_BREP_SHAPE_REPRESENTATION('',(#220),#9487);
#155=ADVANCED_BREP_SHAPE_REPRESENTATION('',(#221),#9488);
#156=ADVANCED_BREP_SHAPE_REPRESENTATION('',(#222,#223,#224,#225,#226,#227,
#228,#229,#230,#231,#232,#233,#234,#235,#236,#237,#238,#239,#240,#241,#242,
#243,#244,#245,#246,#247,#248,#249,#250),#9489);
#157=ADVANCED_BREP_SHAPE_REPRESENTATION('',(#251),#9490);
#158=ADVANCED_BREP_SHAPE_REPRESENTATION('',(#252),#9491);
#159=ADVANCED_BREP_SHAPE_REPRESENTATION('',(#253),#9492);
#160=ADVANCED_BREP_SHAPE_REPRESENTATION('',(#254),#9493);
#161=ADVANCED_BREP_SHAPE_REPRESENTATION('',(#255,#256,#257,#258,#259,#260,
#261,#262,#263,#264,#265,#266,#267,#268,#269,#270,#271,#272,#273,#274,#275),
#9494);
#162=ADVANCED_BREP_SHAPE_REPRESENTATION('',(#276),#9495);
#163=STYLED_ITEM('',(#9593),#220);
#164=STYLED_ITEM('',(#9593),#221);
#165=STYLED_ITEM('',(#9594),#222);
#166=STYLED_ITEM('',(#9594),#223);
#167=STYLED_ITEM('',(#9594),#224);
#168=STYLED_ITEM('',(#9594),#225);
#169=STYLED_ITEM('',(#9594),#226);
#170=STYLED_ITEM('',(#9594),#227);
#171=STYLED_ITEM('',(#9594),#228);
#172=STYLED_ITEM('',(#9594),#229);
#173=STYLED_ITEM('',(#9594),#230);
#174=STYLED_ITEM('',(#9594),#231);
#175=STYLED_ITEM('',(#9594),#232);
#176=STYLED_ITEM('',(#9594),#233);
#177=STYLED_ITEM('',(#9594),#234);
#178=STYLED_ITEM('',(#9594),#235);
#179=STYLED_ITEM('',(#9594),#236);
#180=STYLED_ITEM('',(#9594),#237);
#181=STYLED_ITEM('',(#9594),#238);
#182=STYLED_ITEM('',(#9594),#239);
#183=STYLED_ITEM('',(#9594),#240);
#184=STYLED_ITEM('',(#9594),#241);
#185=STYLED_ITEM('',(#9594),#242);
#186=STYLED_ITEM('',(#9594),#243);
#187=STYLED_ITEM('',(#9594),#244);
#188=STYLED_ITEM('',(#9594),#245);
#189=STYLED_ITEM('',(#9594),#246);
#190=STYLED_ITEM('',(#9594),#247);
#191=STYLED_ITEM('',(#9594),#248);
#192=STYLED_ITEM('',(#9594),#249);
#193=STYLED_ITEM('',(#9594),#250);
#194=STYLED_ITEM('',(#9594),#251);
#195=STYLED_ITEM('',(#9594),#252);
#196=STYLED_ITEM('',(#9594),#253);
#197=STYLED_ITEM('',(#9594),#254);
#198=STYLED_ITEM('',(#9594),#255);
#199=STYLED_ITEM('',(#9594),#256);
#200=STYLED_ITEM('',(#9594),#257);
#201=STYLED_ITEM('',(#9594),#258);
#202=STYLED_ITEM('',(#9594),#259);
#203=STYLED_ITEM('',(#9594),#260);
#204=STYLED_ITEM('',(#9594),#261);
#205=STYLED_ITEM('',(#9594),#262);
#206=STYLED_ITEM('',(#9594),#263);
#207=STYLED_ITEM('',(#9594),#264);
#208=STYLED_ITEM('',(#9594),#265);
#209=STYLED_ITEM('',(#9594),#266);
#210=STYLED_ITEM('',(#9594),#267);
#211=STYLED_ITEM('',(#9594),#268);
#212=STYLED_ITEM('',(#9594),#269);
#213=STYLED_ITEM('',(#9594),#270);
#214=STYLED_ITEM('',(#9594),#271);
#215=STYLED_ITEM('',(#9594),#272);
#216=STYLED_ITEM('',(#9594),#273);
#217=STYLED_ITEM('',(#9594),#274);
#218=STYLED_ITEM('',(#9594),#275);
#219=STYLED_ITEM('',(#9593),#276);
#220=MANIFOLD_SOLID_BREP('Body1',#4965);
#221=MANIFOLD_SOLID_BREP('Body1',#4966);
#222=MANIFOLD_SOLID_BREP('Body1',#4967);
#223=MANIFOLD_SOLID_BREP('Body2',#4968);
#224=MANIFOLD_SOLID_BREP('Body3',#4969);
#225=MANIFOLD_SOLID_BREP('Body4',#4970);
#226=MANIFOLD_SOLID_BREP('Body5',#4971);
#227=MANIFOLD_SOLID_BREP('Body6',#4972);
#228=MANIFOLD_SOLID_BREP('Body7',#4973);
#229=MANIFOLD_SOLID_BREP('Body8',#4974);
#230=MANIFOLD_SOLID_BREP('Body9',#4975);
#231=MANIFOLD_SOLID_BREP('Body10',#4976);
#232=MANIFOLD_SOLID_BREP('Body11',#4977);
#233=MANIFOLD_SOLID_BREP('Body12',#4978);
#234=MANIFOLD_SOLID_BREP('Body13',#4979);
#235=MANIFOLD_SOLID_BREP('Body14',#4980);
#236=MANIFOLD_SOLID_BREP('Body15',#4981);
#237=MANIFOLD_SOLID_BREP('Body16',#4982);
#238=MANIFOLD_SOLID_BREP('Body17',#4983);
#239=MANIFOLD_SOLID_BREP('Body18',#4984);
#240=MANIFOLD_SOLID_BREP('Body19',#4985);
#241=MANIFOLD_SOLID_BREP('Body20',#4986);
#242=MANIFOLD_SOLID_BREP('Body21',#4987);
#243=MANIFOLD_SOLID_BREP('Body22',#4988);
#244=MANIFOLD_SOLID_BREP('Body23',#4989);
#245=MANIFOLD_SOLID_BREP('Body24',#4990);
#246=MANIFOLD_SOLID_BREP('Body25',#4991);
#247=MANIFOLD_SOLID_BREP('Body26',#4992);
#248=MANIFOLD_SOLID_BREP('Body27',#4993);
#249=MANIFOLD_SOLID_BREP('Body28',#4994);
#250=MANIFOLD_SOLID_BREP('Body29',#4995);
#251=MANIFOLD_SOLID_BREP('Body1',#4996);
#252=MANIFOLD_SOLID_BREP('Body1',#4997);
#253=MANIFOLD_SOLID_BREP('Body1',#4998);
#254=MANIFOLD_SOLID_BREP('Body1',#4999);
#255=MANIFOLD_SOLID_BREP('Body1',#5000);
#256=MANIFOLD_SOLID_BREP('Body2',#5001);
#257=MANIFOLD_SOLID_BREP('Body3',#5002);
#258=MANIFOLD_SOLID_BREP('Body4',#5003);
#259=MANIFOLD_SOLID_BREP('Body5',#5004);
#260=MANIFOLD_SOLID_BREP('Body6',#5005);
#261=MANIFOLD_SOLID_BREP('Body7',#5006);
#262=MANIFOLD_SOLID_BREP('Body8',#5007);
#263=MANIFOLD_SOLID_BREP('Body9',#5008);
#264=MANIFOLD_SOLID_BREP('Body10',#5009);
#265=MANIFOLD_SOLID_BREP('Body11',#5010);
#266=MANIFOLD_SOLID_BREP('Body12',#5011);
#267=MANIFOLD_SOLID_BREP('Body13',#5012);
#268=MANIFOLD_SOLID_BREP('Body14',#5013);
#269=MANIFOLD_SOLID_BREP('Body15',#5014);
#270=MANIFOLD_SOLID_BREP('Body16',#5015);
#271=MANIFOLD_SOLID_BREP('Body17',#5016);
#272=MANIFOLD_SOLID_BREP('Body18',#5017);
#273=MANIFOLD_SOLID_BREP('Body19',#5018);
#274=MANIFOLD_SOLID_BREP('Body20',#5019);
#275=MANIFOLD_SOLID_BREP('Body21',#5020);
#276=MANIFOLD_SOLID_BREP('Body1',#5021);
#277=ELLIPSE('',#5185,1.4142135623731,1.);
#278=ELLIPSE('',#5196,1.4142135623731,1.);
#279=SPHERICAL_SURFACE('',#5169,0.999999999999996);
#280=SPHERICAL_SURFACE('',#5173,0.999999999999996);
#281=SPHERICAL_SURFACE('',#5177,0.999999999999996);
#282=SPHERICAL_SURFACE('',#5181,0.999999999999996);
#283=SPHERICAL_SURFACE('',#5186,0.999999999999996);
#284=SPHERICAL_SURFACE('',#5192,0.999999999999996);
#285=SPHERICAL_SURFACE('',#5240,0.999999999999996);
#286=SPHERICAL_SURFACE('',#5244,1.00000000000001);
#287=SPHERICAL_SURFACE('',#5248,1.00000000000001);
#288=SPHERICAL_SURFACE('',#5252,0.999999999999996);
#289=SPHERICAL_SURFACE('',#5257,0.999999999999996);
#290=SPHERICAL_SURFACE('',#5261,0.999999999999996);
#291=SPHERICAL_SURFACE('',#5266,0.999999999999996);
#292=SPHERICAL_SURFACE('',#5272,1.00000000000001);
#293=SPHERICAL_SURFACE('',#5317,1.49484711634153);
#294=SPHERICAL_SURFACE('',#5337,1.49484711634153);
#295=SPHERICAL_SURFACE('',#5339,1.49484711634153);
#296=SPHERICAL_SURFACE('',#5341,1.49484711634153);
#297=SPHERICAL_SURFACE('',#5343,1.49484711634153);
#298=SPHERICAL_SURFACE('',#5345,1.49484711634153);
#299=SPHERICAL_SURFACE('',#5347,1.49484711634153);
#300=SPHERICAL_SURFACE('',#5349,1.49484711634153);
#301=SPHERICAL_SURFACE('',#5351,1.49484711634153);
#302=SPHERICAL_SURFACE('',#5353,1.49484711634153);
#303=SPHERICAL_SURFACE('',#5358,1.49484711634152);
#304=SPHERICAL_SURFACE('',#5367,1.49484711634152);
#305=SPHERICAL_SURFACE('',#5376,1.49484711634152);
#306=SPHERICAL_SURFACE('',#5385,1.49484711634152);
#307=SPHERICAL_SURFACE('',#5394,1.49484711634152);
#308=SPHERICAL_SURFACE('',#5403,1.49484711634152);
#309=SPHERICAL_SURFACE('',#5412,1.49484711634152);
#310=SPHERICAL_SURFACE('',#5421,1.49484711634152);
#311=SPHERICAL_SURFACE('',#5430,1.49484711634152);
#312=SPHERICAL_SURFACE('',#5439,1.49484711634152);
#313=SPHERICAL_SURFACE('',#5456,1.49484711634152);
#314=SPHERICAL_SURFACE('',#5465,1.49484711634152);
#315=SPHERICAL_SURFACE('',#5471,1.49484711634153);
#316=SPHERICAL_SURFACE('',#5473,1.49484711634153);
#317=SPHERICAL_SURFACE('',#5595,2.86797988869785);
#318=SPHERICAL_SURFACE('',#5615,2.86797988869785);
#319=SPHERICAL_SURFACE('',#5617,2.86797988869785);
#320=SPHERICAL_SURFACE('',#5619,2.86797988869785);
#321=SPHERICAL_SURFACE('',#5621,2.86797988869785);
#322=SPHERICAL_SURFACE('',#5623,2.86797988869785);
#323=SPHERICAL_SURFACE('',#5625,2.86797988869785);
#324=SPHERICAL_SURFACE('',#5627,2.86797988869785);
#325=SPHERICAL_SURFACE('',#5633,2.86797988869795);
#326=SPHERICAL_SURFACE('',#5643,2.86797988869795);
#327=SPHERICAL_SURFACE('',#5653,2.86797988869795);
#328=SPHERICAL_SURFACE('',#5663,2.86797988869795);
#329=SPHERICAL_SURFACE('',#5673,2.86797988869795);
#330=SPHERICAL_SURFACE('',#5683,2.86797988869795);
#331=SPHERICAL_SURFACE('',#5693,2.86797988869795);
#332=SPHERICAL_SURFACE('',#5703,2.86797988869795);
#333=FACE_BOUND('',#956,.T.);
#334=FACE_BOUND('',#963,.T.);
#335=FACE_BOUND('',#970,.T.);
#336=FACE_BOUND('',#972,.T.);
#337=FACE_BOUND('',#975,.T.);
#338=FACE_BOUND('',#978,.T.);
#339=FACE_BOUND('',#979,.T.);
#340=FACE_BOUND('',#1000,.T.);
#341=FACE_BOUND('',#1001,.T.);
#342=FACE_BOUND('',#1003,.T.);
#343=FACE_BOUND('',#1011,.T.);
#344=FACE_BOUND('',#1018,.T.);
#345=FACE_BOUND('',#1021,.T.);
#346=FACE_BOUND('',#1045,.T.);
#347=FACE_BOUND('',#1046,.T.);
#348=FACE_BOUND('',#1047,.T.);
#349=FACE_BOUND('',#1050,.T.);
#350=FACE_BOUND('',#1051,.T.);
#351=FACE_BOUND('',#1054,.T.);
#352=FACE_BOUND('',#1055,.T.);
#353=FACE_BOUND('',#1059,.T.);
#354=FACE_BOUND('',#1069,.T.);
#355=FACE_BOUND('',#1071,.T.);
#356=FACE_BOUND('',#1080,.T.);
#357=FACE_BOUND('',#1082,.T.);
#358=FACE_BOUND('',#1094,.T.);
#359=FACE_BOUND('',#1095,.T.);
#360=FACE_BOUND('',#1097,.T.);
#361=FACE_BOUND('',#1099,.T.);
#362=FACE_BOUND('',#1102,.T.);
#363=FACE_BOUND('',#1103,.T.);
#364=FACE_BOUND('',#1105,.T.);
#365=FACE_BOUND('',#1107,.T.);
#366=FACE_BOUND('',#1110,.T.);
#367=FACE_BOUND('',#1111,.T.);
#368=FACE_BOUND('',#1113,.T.);
#369=FACE_BOUND('',#1115,.T.);
#370=FACE_BOUND('',#1118,.T.);
#371=FACE_BOUND('',#1119,.T.);
#372=FACE_BOUND('',#1121,.T.);
#373=FACE_BOUND('',#1123,.T.);
#374=FACE_BOUND('',#1126,.T.);
#375=FACE_BOUND('',#1127,.T.);
#376=FACE_BOUND('',#1129,.T.);
#377=FACE_BOUND('',#1131,.T.);
#378=FACE_BOUND('',#1134,.T.);
#379=FACE_BOUND('',#1135,.T.);
#380=FACE_BOUND('',#1137,.T.);
#381=FACE_BOUND('',#1139,.T.);
#382=FACE_BOUND('',#1142,.T.);
#383=FACE_BOUND('',#1143,.T.);
#384=FACE_BOUND('',#1145,.T.);
#385=FACE_BOUND('',#1147,.T.);
#386=FACE_BOUND('',#1150,.T.);
#387=FACE_BOUND('',#1151,.T.);
#388=FACE_BOUND('',#1153,.T.);
#389=FACE_BOUND('',#1155,.T.);
#390=FACE_BOUND('',#1158,.T.);
#391=FACE_BOUND('',#1159,.T.);
#392=FACE_BOUND('',#1161,.T.);
#393=FACE_BOUND('',#1163,.T.);
#394=FACE_BOUND('',#1166,.T.);
#395=FACE_BOUND('',#1167,.T.);
#396=FACE_BOUND('',#1169,.T.);
#397=FACE_BOUND('',#1171,.T.);
#398=FACE_BOUND('',#1175,.T.);
#399=FACE_BOUND('',#1177,.T.);
#400=FACE_BOUND('',#1180,.T.);
#401=FACE_BOUND('',#1181,.T.);
#402=FACE_BOUND('',#1183,.T.);
#403=FACE_BOUND('',#1185,.T.);
#404=FACE_BOUND('',#1188,.T.);
#405=FACE_BOUND('',#1189,.T.);
#406=FACE_BOUND('',#1191,.T.);
#407=FACE_BOUND('',#1193,.T.);
#408=FACE_BOUND('',#1203,.T.);
#409=FACE_BOUND('',#1205,.T.);
#410=FACE_BOUND('',#1213,.T.);
#411=FACE_BOUND('',#1215,.T.);
#412=FACE_BOUND('',#1219,.T.);
#413=FACE_BOUND('',#1236,.T.);
#414=FACE_BOUND('',#1242,.T.);
#415=FACE_BOUND('',#1245,.T.);
#416=FACE_BOUND('',#1254,.T.);
#417=FACE_BOUND('',#1257,.T.);
#418=FACE_BOUND('',#1265,.T.);
#419=FACE_BOUND('',#1267,.T.);
#420=FACE_BOUND('',#1276,.T.);
#421=FACE_BOUND('',#1278,.T.);
#422=FACE_BOUND('',#1288,.T.);
#423=FACE_BOUND('',#1289,.T.);
#424=FACE_BOUND('',#1291,.T.);
#425=FACE_BOUND('',#1293,.T.);
#426=FACE_BOUND('',#1296,.T.);
#427=FACE_BOUND('',#1297,.T.);
#428=FACE_BOUND('',#1299,.T.);
#429=FACE_BOUND('',#1301,.T.);
#430=FACE_BOUND('',#1304,.T.);
#431=FACE_BOUND('',#1305,.T.);
#432=FACE_BOUND('',#1307,.T.);
#433=FACE_BOUND('',#1309,.T.);
#434=FACE_BOUND('',#1312,.T.);
#435=FACE_BOUND('',#1313,.T.);
#436=FACE_BOUND('',#1315,.T.);
#437=FACE_BOUND('',#1317,.T.);
#438=FACE_BOUND('',#1320,.T.);
#439=FACE_BOUND('',#1321,.T.);
#440=FACE_BOUND('',#1323,.T.);
#441=FACE_BOUND('',#1325,.T.);
#442=FACE_BOUND('',#1328,.T.);
#443=FACE_BOUND('',#1329,.T.);
#444=FACE_BOUND('',#1331,.T.);
#445=FACE_BOUND('',#1333,.T.);
#446=FACE_BOUND('',#1336,.T.);
#447=FACE_BOUND('',#1337,.T.);
#448=FACE_BOUND('',#1339,.T.);
#449=FACE_BOUND('',#1341,.T.);
#450=FACE_BOUND('',#1344,.T.);
#451=FACE_BOUND('',#1345,.T.);
#452=FACE_BOUND('',#1347,.T.);
#453=FACE_BOUND('',#1349,.T.);
#454=FACE_BOUND('',#1353,.T.);
#455=FACE_BOUND('',#1355,.T.);
#456=FACE_BOUND('',#1363,.T.);
#457=FACE_BOUND('',#1365,.T.);
#458=FACE_BOUND('',#1373,.T.);
#459=FACE_BOUND('',#1375,.T.);
#460=FACE_BOUND('',#1388,.T.);
#461=FACE_BOUND('',#1389,.T.);
#462=FACE_BOUND('',#1392,.T.);
#463=FACE_BOUND('',#1393,.T.);
#464=FACE_BOUND('',#1394,.T.);
#465=FACE_BOUND('',#1399,.T.);
#466=FACE_BOUND('',#1400,.T.);
#467=FACE_BOUND('',#1401,.T.);
#468=FACE_BOUND('',#1403,.T.);
#469=FACE_BOUND('',#1404,.T.);
#470=FACE_BOUND('',#1409,.T.);
#471=FACE_BOUND('',#1410,.T.);
#472=FACE_BOUND('',#1416,.T.);
#473=FACE_BOUND('',#1417,.T.);
#474=FACE_BOUND('',#1419,.T.);
#475=FACE_BOUND('',#1420,.T.);
#476=FACE_BOUND('',#1421,.T.);
#477=FACE_BOUND('',#1422,.T.);
#478=FACE_BOUND('',#1424,.T.);
#479=FACE_BOUND('',#1425,.T.);
#480=FACE_BOUND('',#1426,.T.);
#481=FACE_BOUND('',#1427,.T.);
#482=PLANE('',#5127);
#483=PLANE('',#5132);
#484=PLANE('',#5136);
#485=PLANE('',#5140);
#486=PLANE('',#5147);
#487=PLANE('',#5153);
#488=PLANE('',#5154);
#489=PLANE('',#5157);
#490=PLANE('',#5159);
#491=PLANE('',#5164);
#492=PLANE('',#5202);
#493=PLANE('',#5203);
#494=PLANE('',#5206);
#495=PLANE('',#5207);
#496=PLANE('',#5209);
#497=PLANE('',#5212);
#498=PLANE('',#5217);
#499=PLANE('',#5222);
#500=PLANE('',#5226);
#501=PLANE('',#5230);
#502=PLANE('',#5235);
#503=PLANE('',#5284);
#504=PLANE('',#5287);
#505=PLANE('',#5288);
#506=PLANE('',#5289);
#507=PLANE('',#5290);
#508=PLANE('',#5291);
#509=PLANE('',#5294);
#510=PLANE('',#5297);
#511=PLANE('',#5315);
#512=PLANE('',#5316);
#513=PLANE('',#5335);
#514=PLANE('',#5336);
#515=PLANE('',#5362);
#516=PLANE('',#5363);
#517=PLANE('',#5371);
#518=PLANE('',#5372);
#519=PLANE('',#5380);
#520=PLANE('',#5381);
#521=PLANE('',#5389);
#522=PLANE('',#5390);
#523=PLANE('',#5398);
#524=PLANE('',#5399);
#525=PLANE('',#5407);
#526=PLANE('',#5408);
#527=PLANE('',#5416);
#528=PLANE('',#5417);
#529=PLANE('',#5425);
#530=PLANE('',#5426);
#531=PLANE('',#5434);
#532=PLANE('',#5435);
#533=PLANE('',#5443);
#534=PLANE('',#5444);
#535=PLANE('',#5451);
#536=PLANE('',#5452);
#537=PLANE('',#5460);
#538=PLANE('',#5461);
#539=PLANE('',#5469);
#540=PLANE('',#5470);
#541=PLANE('',#5494);
#542=PLANE('',#5495);
#543=PLANE('',#5513);
#544=PLANE('',#5514);
#545=PLANE('',#5523);
#546=PLANE('',#5526);
#547=PLANE('',#5527);
#548=PLANE('',#5528);
#549=PLANE('',#5529);
#550=PLANE('',#5530);
#551=PLANE('',#5531);
#552=PLANE('',#5532);
#553=PLANE('',#5533);
#554=PLANE('',#5534);
#555=PLANE('',#5535);
#556=PLANE('',#5536);
#557=PLANE('',#5537);
#558=PLANE('',#5540);
#559=PLANE('',#5541);
#560=PLANE('',#5546);
#561=PLANE('',#5550);
#562=PLANE('',#5551);
#563=PLANE('',#5555);
#564=PLANE('',#5557);
#565=PLANE('',#5561);
#566=PLANE('',#5566);
#567=PLANE('',#5570);
#568=PLANE('',#5571);
#569=PLANE('',#5575);
#570=PLANE('',#5593);
#571=PLANE('',#5594);
#572=PLANE('',#5613);
#573=PLANE('',#5614);
#574=PLANE('',#5637);
#575=PLANE('',#5638);
#576=PLANE('',#5647);
#577=PLANE('',#5648);
#578=PLANE('',#5657);
#579=PLANE('',#5658);
#580=PLANE('',#5667);
#581=PLANE('',#5668);
#582=PLANE('',#5677);
#583=PLANE('',#5678);
#584=PLANE('',#5687);
#585=PLANE('',#5688);
#586=PLANE('',#5697);
#587=PLANE('',#5698);
#588=PLANE('',#5707);
#589=PLANE('',#5708);
#590=PLANE('',#5715);
#591=PLANE('',#5716);
#592=PLANE('',#5736);
#593=PLANE('',#5737);
#594=PLANE('',#5755);
#595=PLANE('',#5756);
#596=PLANE('',#5774);
#597=PLANE('',#5775);
#598=PLANE('',#5776);
#599=PLANE('',#5777);
#600=PLANE('',#5778);
#601=PLANE('',#5779);
#602=PLANE('',#5783);
#603=PLANE('',#5784);
#604=PLANE('',#5785);
#605=PLANE('',#5786);
#606=PLANE('',#5790);
#607=PLANE('',#5791);
#608=PLANE('',#5792);
#609=PLANE('',#5793);
#610=PLANE('',#5794);
#611=PLANE('',#5795);
#612=PLANE('',#5796);
#613=PLANE('',#5797);
#614=PLANE('',#5798);
#615=PLANE('',#5799);
#616=PLANE('',#5803);
#617=PLANE('',#5804);
#618=PLANE('',#5805);
#619=PLANE('',#5806);
#620=PLANE('',#5807);
#621=PLANE('',#5808);
#622=FACE_OUTER_BOUND('',#954,.T.);
#623=FACE_OUTER_BOUND('',#955,.T.);
#624=FACE_OUTER_BOUND('',#957,.T.);
#625=FACE_OUTER_BOUND('',#958,.T.);
#626=FACE_OUTER_BOUND('',#959,.T.);
#627=FACE_OUTER_BOUND('',#960,.T.);
#628=FACE_OUTER_BOUND('',#961,.T.);
#629=FACE_OUTER_BOUND('',#962,.T.);
#630=FACE_OUTER_BOUND('',#964,.T.);
#631=FACE_OUTER_BOUND('',#965,.T.);
#632=FACE_OUTER_BOUND('',#966,.T.);
#633=FACE_OUTER_BOUND('',#967,.T.);
#634=FACE_OUTER_BOUND('',#968,.T.);
#635=FACE_OUTER_BOUND('',#969,.T.);
#636=FACE_OUTER_BOUND('',#971,.T.);
#637=FACE_OUTER_BOUND('',#973,.T.);
#638=FACE_OUTER_BOUND('',#974,.T.);
#639=FACE_OUTER_BOUND('',#976,.T.);
#640=FACE_OUTER_BOUND('',#977,.T.);
#641=FACE_OUTER_BOUND('',#980,.T.);
#642=FACE_OUTER_BOUND('',#981,.T.);
#643=FACE_OUTER_BOUND('',#982,.T.);
#644=FACE_OUTER_BOUND('',#983,.T.);
#645=FACE_OUTER_BOUND('',#984,.T.);
#646=FACE_OUTER_BOUND('',#985,.T.);
#647=FACE_OUTER_BOUND('',#986,.T.);
#648=FACE_OUTER_BOUND('',#987,.T.);
#649=FACE_OUTER_BOUND('',#988,.T.);
#650=FACE_OUTER_BOUND('',#989,.T.);
#651=FACE_OUTER_BOUND('',#990,.T.);
#652=FACE_OUTER_BOUND('',#991,.T.);
#653=FACE_OUTER_BOUND('',#992,.T.);
#654=FACE_OUTER_BOUND('',#993,.T.);
#655=FACE_OUTER_BOUND('',#994,.T.);
#656=FACE_OUTER_BOUND('',#995,.T.);
#657=FACE_OUTER_BOUND('',#996,.T.);
#658=FACE_OUTER_BOUND('',#997,.T.);
#659=FACE_OUTER_BOUND('',#998,.T.);
#660=FACE_OUTER_BOUND('',#999,.T.);
#661=FACE_OUTER_BOUND('',#1002,.T.);
#662=FACE_OUTER_BOUND('',#1004,.T.);
#663=FACE_OUTER_BOUND('',#1005,.T.);
#664=FACE_OUTER_BOUND('',#1006,.T.);
#665=FACE_OUTER_BOUND('',#1007,.T.);
#666=FACE_OUTER_BOUND('',#1008,.T.);
#667=FACE_OUTER_BOUND('',#1009,.T.);
#668=FACE_OUTER_BOUND('',#1010,.T.);
#669=FACE_OUTER_BOUND('',#1012,.T.);
#670=FACE_OUTER_BOUND('',#1013,.T.);
#671=FACE_OUTER_BOUND('',#1014,.T.);
#672=FACE_OUTER_BOUND('',#1015,.T.);
#673=FACE_OUTER_BOUND('',#1016,.T.);
#674=FACE_OUTER_BOUND('',#1017,.T.);
#675=FACE_OUTER_BOUND('',#1019,.T.);
#676=FACE_OUTER_BOUND('',#1020,.T.);
#677=FACE_OUTER_BOUND('',#1022,.T.);
#678=FACE_OUTER_BOUND('',#1023,.T.);
#679=FACE_OUTER_BOUND('',#1024,.T.);
#680=FACE_OUTER_BOUND('',#1025,.T.);
#681=FACE_OUTER_BOUND('',#1026,.T.);
#682=FACE_OUTER_BOUND('',#1027,.T.);
#683=FACE_OUTER_BOUND('',#1028,.T.);
#684=FACE_OUTER_BOUND('',#1029,.T.);
#685=FACE_OUTER_BOUND('',#1030,.T.);
#686=FACE_OUTER_BOUND('',#1031,.T.);
#687=FACE_OUTER_BOUND('',#1032,.T.);
#688=FACE_OUTER_BOUND('',#1033,.T.);
#689=FACE_OUTER_BOUND('',#1034,.T.);
#690=FACE_OUTER_BOUND('',#1035,.T.);
#691=FACE_OUTER_BOUND('',#1036,.T.);
#692=FACE_OUTER_BOUND('',#1037,.T.);
#693=FACE_OUTER_BOUND('',#1038,.T.);
#694=FACE_OUTER_BOUND('',#1039,.T.);
#695=FACE_OUTER_BOUND('',#1040,.T.);
#696=FACE_OUTER_BOUND('',#1041,.T.);
#697=FACE_OUTER_BOUND('',#1042,.T.);
#698=FACE_OUTER_BOUND('',#1043,.T.);
#699=FACE_OUTER_BOUND('',#1044,.T.);
#700=FACE_OUTER_BOUND('',#1048,.T.);
#701=FACE_OUTER_BOUND('',#1049,.T.);
#702=FACE_OUTER_BOUND('',#1052,.T.);
#703=FACE_OUTER_BOUND('',#1053,.T.);
#704=FACE_OUTER_BOUND('',#1056,.T.);
#705=FACE_OUTER_BOUND('',#1057,.T.);
#706=FACE_OUTER_BOUND('',#1058,.T.);
#707=FACE_OUTER_BOUND('',#1060,.T.);
#708=FACE_OUTER_BOUND('',#1061,.T.);
#709=FACE_OUTER_BOUND('',#1062,.T.);
#710=FACE_OUTER_BOUND('',#1063,.T.);
#711=FACE_OUTER_BOUND('',#1064,.T.);
#712=FACE_OUTER_BOUND('',#1065,.T.);
#713=FACE_OUTER_BOUND('',#1066,.T.);
#714=FACE_OUTER_BOUND('',#1067,.T.);
#715=FACE_OUTER_BOUND('',#1068,.T.);
#716=FACE_OUTER_BOUND('',#1070,.T.);
#717=FACE_OUTER_BOUND('',#1072,.T.);
#718=FACE_OUTER_BOUND('',#1073,.T.);
#719=FACE_OUTER_BOUND('',#1074,.T.);
#720=FACE_OUTER_BOUND('',#1075,.T.);
#721=FACE_OUTER_BOUND('',#1076,.T.);
#722=FACE_OUTER_BOUND('',#1077,.T.);
#723=FACE_OUTER_BOUND('',#1078,.T.);
#724=FACE_OUTER_BOUND('',#1079,.T.);
#725=FACE_OUTER_BOUND('',#1081,.T.);
#726=FACE_OUTER_BOUND('',#1083,.T.);
#727=FACE_OUTER_BOUND('',#1084,.T.);
#728=FACE_OUTER_BOUND('',#1085,.T.);
#729=FACE_OUTER_BOUND('',#1086,.T.);
#730=FACE_OUTER_BOUND('',#1087,.T.);
#731=FACE_OUTER_BOUND('',#1088,.T.);
#732=FACE_OUTER_BOUND('',#1089,.T.);
#733=FACE_OUTER_BOUND('',#1090,.T.);
#734=FACE_OUTER_BOUND('',#1091,.T.);
#735=FACE_OUTER_BOUND('',#1092,.T.);
#736=FACE_OUTER_BOUND('',#1093,.T.);
#737=FACE_OUTER_BOUND('',#1096,.T.);
#738=FACE_OUTER_BOUND('',#1098,.T.);
#739=FACE_OUTER_BOUND('',#1100,.T.);
#740=FACE_OUTER_BOUND('',#1101,.T.);
#741=FACE_OUTER_BOUND('',#1104,.T.);
#742=FACE_OUTER_BOUND('',#1106,.T.);
#743=FACE_OUTER_BOUND('',#1108,.T.);
#744=FACE_OUTER_BOUND('',#1109,.T.);
#745=FACE_OUTER_BOUND('',#1112,.T.);
#746=FACE_OUTER_BOUND('',#1114,.T.);
#747=FACE_OUTER_BOUND('',#1116,.T.);
#748=FACE_OUTER_BOUND('',#1117,.T.);
#749=FACE_OUTER_BOUND('',#1120,.T.);
#750=FACE_OUTER_BOUND('',#1122,.T.);
#751=FACE_OUTER_BOUND('',#1124,.T.);
#752=FACE_OUTER_BOUND('',#1125,.T.);
#753=FACE_OUTER_BOUND('',#1128,.T.);
#754=FACE_OUTER_BOUND('',#1130,.T.);
#755=FACE_OUTER_BOUND('',#1132,.T.);
#756=FACE_OUTER_BOUND('',#1133,.T.);
#757=FACE_OUTER_BOUND('',#1136,.T.);
#758=FACE_OUTER_BOUND('',#1138,.T.);
#759=FACE_OUTER_BOUND('',#1140,.T.);
#760=FACE_OUTER_BOUND('',#1141,.T.);
#761=FACE_OUTER_BOUND('',#1144,.T.);
#762=FACE_OUTER_BOUND('',#1146,.T.);
#763=FACE_OUTER_BOUND('',#1148,.T.);
#764=FACE_OUTER_BOUND('',#1149,.T.);
#765=FACE_OUTER_BOUND('',#1152,.T.);
#766=FACE_OUTER_BOUND('',#1154,.T.);
#767=FACE_OUTER_BOUND('',#1156,.T.);
#768=FACE_OUTER_BOUND('',#1157,.T.);
#769=FACE_OUTER_BOUND('',#1160,.T.);
#770=FACE_OUTER_BOUND('',#1162,.T.);
#771=FACE_OUTER_BOUND('',#1164,.T.);
#772=FACE_OUTER_BOUND('',#1165,.T.);
#773=FACE_OUTER_BOUND('',#1168,.T.);
#774=FACE_OUTER_BOUND('',#1170,.T.);
#775=FACE_OUTER_BOUND('',#1172,.T.);
#776=FACE_OUTER_BOUND('',#1173,.T.);
#777=FACE_OUTER_BOUND('',#1174,.T.);
#778=FACE_OUTER_BOUND('',#1176,.T.);
#779=FACE_OUTER_BOUND('',#1178,.T.);
#780=FACE_OUTER_BOUND('',#1179,.T.);
#781=FACE_OUTER_BOUND('',#1182,.T.);
#782=FACE_OUTER_BOUND('',#1184,.T.);
#783=FACE_OUTER_BOUND('',#1186,.T.);
#784=FACE_OUTER_BOUND('',#1187,.T.);
#785=FACE_OUTER_BOUND('',#1190,.T.);
#786=FACE_OUTER_BOUND('',#1192,.T.);
#787=FACE_OUTER_BOUND('',#1194,.T.);
#788=FACE_OUTER_BOUND('',#1195,.T.);
#789=FACE_OUTER_BOUND('',#1196,.T.);
#790=FACE_OUTER_BOUND('',#1197,.T.);
#791=FACE_OUTER_BOUND('',#1198,.T.);
#792=FACE_OUTER_BOUND('',#1199,.T.);
#793=FACE_OUTER_BOUND('',#1200,.T.);
#794=FACE_OUTER_BOUND('',#1201,.T.);
#795=FACE_OUTER_BOUND('',#1202,.T.);
#796=FACE_OUTER_BOUND('',#1204,.T.);
#797=FACE_OUTER_BOUND('',#1206,.T.);
#798=FACE_OUTER_BOUND('',#1207,.T.);
#799=FACE_OUTER_BOUND('',#1208,.T.);
#800=FACE_OUTER_BOUND('',#1209,.T.);
#801=FACE_OUTER_BOUND('',#1210,.T.);
#802=FACE_OUTER_BOUND('',#1211,.T.);
#803=FACE_OUTER_BOUND('',#1212,.T.);
#804=FACE_OUTER_BOUND('',#1214,.T.);
#805=FACE_OUTER_BOUND('',#1216,.T.);
#806=FACE_OUTER_BOUND('',#1217,.T.);
#807=FACE_OUTER_BOUND('',#1218,.T.);
#808=FACE_OUTER_BOUND('',#1220,.T.);
#809=FACE_OUTER_BOUND('',#1221,.T.);
#810=FACE_OUTER_BOUND('',#1222,.T.);
#811=FACE_OUTER_BOUND('',#1223,.T.);
#812=FACE_OUTER_BOUND('',#1224,.T.);
#813=FACE_OUTER_BOUND('',#1225,.T.);
#814=FACE_OUTER_BOUND('',#1226,.T.);
#815=FACE_OUTER_BOUND('',#1227,.T.);
#816=FACE_OUTER_BOUND('',#1228,.T.);
#817=FACE_OUTER_BOUND('',#1229,.T.);
#818=FACE_OUTER_BOUND('',#1230,.T.);
#819=FACE_OUTER_BOUND('',#1231,.T.);
#820=FACE_OUTER_BOUND('',#1232,.T.);
#821=FACE_OUTER_BOUND('',#1233,.T.);
#822=FACE_OUTER_BOUND('',#1234,.T.);
#823=FACE_OUTER_BOUND('',#1235,.T.);
#824=FACE_OUTER_BOUND('',#1237,.T.);
#825=FACE_OUTER_BOUND('',#1238,.T.);
#826=FACE_OUTER_BOUND('',#1239,.T.);
#827=FACE_OUTER_BOUND('',#1240,.T.);
#828=FACE_OUTER_BOUND('',#1241,.T.);
#829=FACE_OUTER_BOUND('',#1243,.T.);
#830=FACE_OUTER_BOUND('',#1244,.T.);
#831=FACE_OUTER_BOUND('',#1246,.T.);
#832=FACE_OUTER_BOUND('',#1247,.T.);
#833=FACE_OUTER_BOUND('',#1248,.T.);
#834=FACE_OUTER_BOUND('',#1249,.T.);
#835=FACE_OUTER_BOUND('',#1250,.T.);
#836=FACE_OUTER_BOUND('',#1251,.T.);
#837=FACE_OUTER_BOUND('',#1252,.T.);
#838=FACE_OUTER_BOUND('',#1253,.T.);
#839=FACE_OUTER_BOUND('',#1255,.T.);
#840=FACE_OUTER_BOUND('',#1256,.T.);
#841=FACE_OUTER_BOUND('',#1258,.T.);
#842=FACE_OUTER_BOUND('',#1259,.T.);
#843=FACE_OUTER_BOUND('',#1260,.T.);
#844=FACE_OUTER_BOUND('',#1261,.T.);
#845=FACE_OUTER_BOUND('',#1262,.T.);
#846=FACE_OUTER_BOUND('',#1263,.T.);
#847=FACE_OUTER_BOUND('',#1264,.T.);
#848=FACE_OUTER_BOUND('',#1266,.T.);
#849=FACE_OUTER_BOUND('',#1268,.T.);
#850=FACE_OUTER_BOUND('',#1269,.T.);
#851=FACE_OUTER_BOUND('',#1270,.T.);
#852=FACE_OUTER_BOUND('',#1271,.T.);
#853=FACE_OUTER_BOUND('',#1272,.T.);
#854=FACE_OUTER_BOUND('',#1273,.T.);
#855=FACE_OUTER_BOUND('',#1274,.T.);
#856=FACE_OUTER_BOUND('',#1275,.T.);
#857=FACE_OUTER_BOUND('',#1277,.T.);
#858=FACE_OUTER_BOUND('',#1279,.T.);
#859=FACE_OUTER_BOUND('',#1280,.T.);
#860=FACE_OUTER_BOUND('',#1281,.T.);
#861=FACE_OUTER_BOUND('',#1282,.T.);
#862=FACE_OUTER_BOUND('',#1283,.T.);
#863=FACE_OUTER_BOUND('',#1284,.T.);
#864=FACE_OUTER_BOUND('',#1285,.T.);
#865=FACE_OUTER_BOUND('',#1286,.T.);
#866=FACE_OUTER_BOUND('',#1287,.T.);
#867=FACE_OUTER_BOUND('',#1290,.T.);
#868=FACE_OUTER_BOUND('',#1292,.T.);
#869=FACE_OUTER_BOUND('',#1294,.T.);
#870=FACE_OUTER_BOUND('',#1295,.T.);
#871=FACE_OUTER_BOUND('',#1298,.T.);
#872=FACE_OUTER_BOUND('',#1300,.T.);
#873=FACE_OUTER_BOUND('',#1302,.T.);
#874=FACE_OUTER_BOUND('',#1303,.T.);
#875=FACE_OUTER_BOUND('',#1306,.T.);
#876=FACE_OUTER_BOUND('',#1308,.T.);
#877=FACE_OUTER_BOUND('',#1310,.T.);
#878=FACE_OUTER_BOUND('',#1311,.T.);
#879=FACE_OUTER_BOUND('',#1314,.T.);
#880=FACE_OUTER_BOUND('',#1316,.T.);
#881=FACE_OUTER_BOUND('',#1318,.T.);
#882=FACE_OUTER_BOUND('',#1319,.T.);
#883=FACE_OUTER_BOUND('',#1322,.T.);
#884=FACE_OUTER_BOUND('',#1324,.T.);
#885=FACE_OUTER_BOUND('',#1326,.T.);
#886=FACE_OUTER_BOUND('',#1327,.T.);
#887=FACE_OUTER_BOUND('',#1330,.T.);
#888=FACE_OUTER_BOUND('',#1332,.T.);
#889=FACE_OUTER_BOUND('',#1334,.T.);
#890=FACE_OUTER_BOUND('',#1335,.T.);
#891=FACE_OUTER_BOUND('',#1338,.T.);
#892=FACE_OUTER_BOUND('',#1340,.T.);
#893=FACE_OUTER_BOUND('',#1342,.T.);
#894=FACE_OUTER_BOUND('',#1343,.T.);
#895=FACE_OUTER_BOUND('',#1346,.T.);
#896=FACE_OUTER_BOUND('',#1348,.T.);
#897=FACE_OUTER_BOUND('',#1350,.T.);
#898=FACE_OUTER_BOUND('',#1351,.T.);
#899=FACE_OUTER_BOUND('',#1352,.T.);
#900=FACE_OUTER_BOUND('',#1354,.T.);
#901=FACE_OUTER_BOUND('',#1356,.T.);
#902=FACE_OUTER_BOUND('',#1357,.T.);
#903=FACE_OUTER_BOUND('',#1358,.T.);
#904=FACE_OUTER_BOUND('',#1359,.T.);
#905=FACE_OUTER_BOUND('',#1360,.T.);
#906=FACE_OUTER_BOUND('',#1361,.T.);
#907=FACE_OUTER_BOUND('',#1362,.T.);
#908=FACE_OUTER_BOUND('',#1364,.T.);
#909=FACE_OUTER_BOUND('',#1366,.T.);
#910=FACE_OUTER_BOUND('',#1367,.T.);
#911=FACE_OUTER_BOUND('',#1368,.T.);
#912=FACE_OUTER_BOUND('',#1369,.T.);
#913=FACE_OUTER_BOUND('',#1370,.T.);
#914=FACE_OUTER_BOUND('',#1371,.T.);
#915=FACE_OUTER_BOUND('',#1372,.T.);
#916=FACE_OUTER_BOUND('',#1374,.T.);
#917=FACE_OUTER_BOUND('',#1376,.T.);
#918=FACE_OUTER_BOUND('',#1377,.T.);
#919=FACE_OUTER_BOUND('',#1378,.T.);
#920=FACE_OUTER_BOUND('',#1379,.T.);
#921=FACE_OUTER_BOUND('',#1380,.T.);
#922=FACE_OUTER_BOUND('',#1381,.T.);
#923=FACE_OUTER_BOUND('',#1382,.T.);
#924=FACE_OUTER_BOUND('',#1383,.T.);
#925=FACE_OUTER_BOUND('',#1384,.T.);
#926=FACE_OUTER_BOUND('',#1385,.T.);
#927=FACE_OUTER_BOUND('',#1386,.T.);
#928=FACE_OUTER_BOUND('',#1387,.T.);
#929=FACE_OUTER_BOUND('',#1390,.T.);
#930=FACE_OUTER_BOUND('',#1391,.T.);
#931=FACE_OUTER_BOUND('',#1395,.T.);
#932=FACE_OUTER_BOUND('',#1396,.T.);
#933=FACE_OUTER_BOUND('',#1397,.T.);
#934=FACE_OUTER_BOUND('',#1398,.T.);
#935=FACE_OUTER_BOUND('',#1402,.T.);
#936=FACE_OUTER_BOUND('',#1405,.T.);
#937=FACE_OUTER_BOUND('',#1406,.T.);
#938=FACE_OUTER_BOUND('',#1407,.T.);
#939=FACE_OUTER_BOUND('',#1408,.T.);
#940=FACE_OUTER_BOUND('',#1411,.T.);
#941=FACE_OUTER_BOUND('',#1412,.T.);
#942=FACE_OUTER_BOUND('',#1413,.T.);
#943=FACE_OUTER_BOUND('',#1414,.T.);
#944=FACE_OUTER_BOUND('',#1415,.T.);
#945=FACE_OUTER_BOUND('',#1418,.T.);
#946=FACE_OUTER_BOUND('',#1423,.T.);
#947=FACE_OUTER_BOUND('',#1428,.T.);
#948=FACE_OUTER_BOUND('',#1429,.T.);
#949=FACE_OUTER_BOUND('',#1430,.T.);
#950=FACE_OUTER_BOUND('',#1431,.T.);
#951=FACE_OUTER_BOUND('',#1432,.T.);
#952=FACE_OUTER_BOUND('',#1433,.T.);
#953=FACE_OUTER_BOUND('',#1434,.T.);
#954=EDGE_LOOP('',(#3325,#3326,#3327,#3328));
#955=EDGE_LOOP('',(#3329));
#956=EDGE_LOOP('',(#3330));
#957=EDGE_LOOP('',(#3331,#3332,#3333,#3334));
#958=EDGE_LOOP('',(#3335));
#959=EDGE_LOOP('',(#3336,#3337,#3338,#3339));
#960=EDGE_LOOP('',(#3340));
#961=EDGE_LOOP('',(#3341,#3342,#3343,#3344));
#962=EDGE_LOOP('',(#3345));
#963=EDGE_LOOP('',(#3346));
#964=EDGE_LOOP('',(#3347,#3348,#3349,#3350));
#965=EDGE_LOOP('',(#3351,#3352,#3353,#3354));
#966=EDGE_LOOP('',(#3355));
#967=EDGE_LOOP('',(#3356,#3357,#3358,#3359));
#968=EDGE_LOOP('',(#3360,#3361,#3362,#3363));
#969=EDGE_LOOP('',(#3364,#3365,#3366,#3367,#3368,#3369,#3370,#3371));
#970=EDGE_LOOP('',(#3372));
#971=EDGE_LOOP('',(#3373,#3374,#3375,#3376,#3377,#3378,#3379,#3380));
#972=EDGE_LOOP('',(#3381));
#973=EDGE_LOOP('',(#3382,#3383,#3384,#3385));
#974=EDGE_LOOP('',(#3386,#3387,#3388,#3389,#3390,#3391,#3392,#3393));
#975=EDGE_LOOP('',(#3394));
#976=EDGE_LOOP('',(#3395,#3396,#3397,#3398));
#977=EDGE_LOOP('',(#3399,#3400,#3401,#3402));
#978=EDGE_LOOP('',(#3403));
#979=EDGE_LOOP('',(#3404));
#980=EDGE_LOOP('',(#3405,#3406,#3407,#3408));
#981=EDGE_LOOP('',(#3409,#3410,#3411,#3412));
#982=EDGE_LOOP('',(#3413,#3414,#3415));
#983=EDGE_LOOP('',(#3416,#3417,#3418));
#984=EDGE_LOOP('',(#3419,#3420,#3421,#3422));
#985=EDGE_LOOP('',(#3423,#3424,#3425));
#986=EDGE_LOOP('',(#3426,#3427,#3428));
#987=EDGE_LOOP('',(#3429,#3430,#3431,#3432));
#988=EDGE_LOOP('',(#3433,#3434,#3435));
#989=EDGE_LOOP('',(#3436,#3437,#3438,#3439));
#990=EDGE_LOOP('',(#3440,#3441,#3442,#3443));
#991=EDGE_LOOP('',(#3444,#3445,#3446));
#992=EDGE_LOOP('',(#3447,#3448,#3449,#3450));
#993=EDGE_LOOP('',(#3451,#3452,#3453,#3454));
#994=EDGE_LOOP('',(#3455,#3456,#3457,#3458));
#995=EDGE_LOOP('',(#3459,#3460,#3461,#3462));
#996=EDGE_LOOP('',(#3463,#3464,#3465,#3466));
#997=EDGE_LOOP('',(#3467,#3468,#3469,#3470));
#998=EDGE_LOOP('',(#3471,#3472,#3473,#3474));
#999=EDGE_LOOP('',(#3475,#3476,#3477,#3478,#3479,#3480,#3481,#3482));
#1000=EDGE_LOOP('',(#3483));
#1001=EDGE_LOOP('',(#3484));
#1002=EDGE_LOOP('',(#3485,#3486,#3487,#3488));
#1003=EDGE_LOOP('',(#3489));
#1004=EDGE_LOOP('',(#3490,#3491,#3492,#3493));
#1005=EDGE_LOOP('',(#3494,#3495,#3496,#3497));
#1006=EDGE_LOOP('',(#3498));
#1007=EDGE_LOOP('',(#3499,#3500,#3501,#3502));
#1008=EDGE_LOOP('',(#3503,#3504,#3505,#3506));
#1009=EDGE_LOOP('',(#3507,#3508,#3509,#3510));
#1010=EDGE_LOOP('',(#3511));
#1011=EDGE_LOOP('',(#3512));
#1012=EDGE_LOOP('',(#3513,#3514,#3515,#3516));
#1013=EDGE_LOOP('',(#3517));
#1014=EDGE_LOOP('',(#3518,#3519,#3520,#3521));
#1015=EDGE_LOOP('',(#3522));
#1016=EDGE_LOOP('',(#3523,#3524,#3525,#3526));
#1017=EDGE_LOOP('',(#3527));
#1018=EDGE_LOOP('',(#3528));
#1019=EDGE_LOOP('',(#3529,#3530,#3531,#3532));
#1020=EDGE_LOOP('',(#3533));
#1021=EDGE_LOOP('',(#3534));
#1022=EDGE_LOOP('',(#3535,#3536,#3537,#3538));
#1023=EDGE_LOOP('',(#3539,#3540,#3541,#3542));
#1024=EDGE_LOOP('',(#3543,#3544,#3545));
#1025=EDGE_LOOP('',(#3546,#3547,#3548));
#1026=EDGE_LOOP('',(#3549,#3550,#3551));
#1027=EDGE_LOOP('',(#3552,#3553,#3554));
#1028=EDGE_LOOP('',(#3555,#3556,#3557,#3558));
#1029=EDGE_LOOP('',(#3559,#3560,#3561));
#1030=EDGE_LOOP('',(#3562,#3563,#3564));
#1031=EDGE_LOOP('',(#3565,#3566,#3567,#3568));
#1032=EDGE_LOOP('',(#3569,#3570,#3571));
#1033=EDGE_LOOP('',(#3572,#3573,#3574,#3575));
#1034=EDGE_LOOP('',(#3576,#3577,#3578,#3579));
#1035=EDGE_LOOP('',(#3580,#3581,#3582));
#1036=EDGE_LOOP('',(#3583,#3584,#3585,#3586));
#1037=EDGE_LOOP('',(#3587,#3588,#3589,#3590));
#1038=EDGE_LOOP('',(#3591,#3592,#3593,#3594));
#1039=EDGE_LOOP('',(#3595,#3596,#3597,#3598));
#1040=EDGE_LOOP('',(#3599,#3600,#3601,#3602));
#1041=EDGE_LOOP('',(#3603,#3604,#3605,#3606));
#1042=EDGE_LOOP('',(#3607,#3608,#3609,#3610));
#1043=EDGE_LOOP('',(#3611,#3612,#3613,#3614));
#1044=EDGE_LOOP('',(#3615,#3616,#3617,#3618));
#1045=EDGE_LOOP('',(#3619));
#1046=EDGE_LOOP('',(#3620));
#1047=EDGE_LOOP('',(#3621));
#1048=EDGE_LOOP('',(#3622,#3623,#3624,#3625));
#1049=EDGE_LOOP('',(#3626,#3627,#3628,#3629));
#1050=EDGE_LOOP('',(#3630));
#1051=EDGE_LOOP('',(#3631));
#1052=EDGE_LOOP('',(#3632,#3633,#3634,#3635));
#1053=EDGE_LOOP('',(#3636,#3637,#3638,#3639));
#1054=EDGE_LOOP('',(#3640));
#1055=EDGE_LOOP('',(#3641));
#1056=EDGE_LOOP('',(#3642,#3643,#3644,#3645));
#1057=EDGE_LOOP('',(#3646,#3647,#3648,#3649));
#1058=EDGE_LOOP('',(#3650));
#1059=EDGE_LOOP('',(#3651));
#1060=EDGE_LOOP('',(#3652,#3653,#3654,#3655));
#1061=EDGE_LOOP('',(#3656));
#1062=EDGE_LOOP('',(#3657,#3658,#3659,#3660));
#1063=EDGE_LOOP('',(#3661,#3662,#3663,#3664));
#1064=EDGE_LOOP('',(#3665,#3666,#3667,#3668,#3669));
#1065=EDGE_LOOP('',(#3670,#3671,#3672,#3673,#3674));
#1066=EDGE_LOOP('',(#3675,#3676,#3677,#3678));
#1067=EDGE_LOOP('',(#3679,#3680,#3681,#3682));
#1068=EDGE_LOOP('',(#3683));
#1069=EDGE_LOOP('',(#3684));
#1070=EDGE_LOOP('',(#3685));
#1071=EDGE_LOOP('',(#3686));
#1072=EDGE_LOOP('',(#3687,#3688));
#1073=EDGE_LOOP('',(#3689,#3690,#3691,#3692));
#1074=EDGE_LOOP('',(#3693,#3694,#3695,#3696));
#1075=EDGE_LOOP('',(#3697,#3698,#3699,#3700));
#1076=EDGE_LOOP('',(#3701,#3702,#3703,#3704));
#1077=EDGE_LOOP('',(#3705,#3706,#3707,#3708,#3709));
#1078=EDGE_LOOP('',(#3710,#3711,#3712,#3713,#3714));
#1079=EDGE_LOOP('',(#3715));
#1080=EDGE_LOOP('',(#3716));
#1081=EDGE_LOOP('',(#3717));
#1082=EDGE_LOOP('',(#3718));
#1083=EDGE_LOOP('',(#3719,#3720));
#1084=EDGE_LOOP('',(#3721,#3722));
#1085=EDGE_LOOP('',(#3723,#3724));
#1086=EDGE_LOOP('',(#3725,#3726));
#1087=EDGE_LOOP('',(#3727,#3728));
#1088=EDGE_LOOP('',(#3729,#3730));
#1089=EDGE_LOOP('',(#3731,#3732));
#1090=EDGE_LOOP('',(#3733,#3734));
#1091=EDGE_LOOP('',(#3735,#3736));
#1092=EDGE_LOOP('',(#3737,#3738,#3739,#3740));
#1093=EDGE_LOOP('',(#3741,#3742));
#1094=EDGE_LOOP('',(#3743));
#1095=EDGE_LOOP('',(#3744));
#1096=EDGE_LOOP('',(#3745));
#1097=EDGE_LOOP('',(#3746));
#1098=EDGE_LOOP('',(#3747));
#1099=EDGE_LOOP('',(#3748));
#1100=EDGE_LOOP('',(#3749,#3750,#3751,#3752));
#1101=EDGE_LOOP('',(#3753,#3754));
#1102=EDGE_LOOP('',(#3755));
#1103=EDGE_LOOP('',(#3756));
#1104=EDGE_LOOP('',(#3757));
#1105=EDGE_LOOP('',(#3758));
#1106=EDGE_LOOP('',(#3759));
#1107=EDGE_LOOP('',(#3760));
#1108=EDGE_LOOP('',(#3761,#3762,#3763,#3764));
#1109=EDGE_LOOP('',(#3765,#3766));
#1110=EDGE_LOOP('',(#3767));
#1111=EDGE_LOOP('',(#3768));
#1112=EDGE_LOOP('',(#3769));
#1113=EDGE_LOOP('',(#3770));
#1114=EDGE_LOOP('',(#3771));
#1115=EDGE_LOOP('',(#3772));
#1116=EDGE_LOOP('',(#3773,#3774,#3775,#3776));
#1117=EDGE_LOOP('',(#3777,#3778));
#1118=EDGE_LOOP('',(#3779));
#1119=EDGE_LOOP('',(#3780));
#1120=EDGE_LOOP('',(#3781));
#1121=EDGE_LOOP('',(#3782));
#1122=EDGE_LOOP('',(#3783));
#1123=EDGE_LOOP('',(#3784));
#1124=EDGE_LOOP('',(#3785,#3786,#3787,#3788));
#1125=EDGE_LOOP('',(#3789,#3790));
#1126=EDGE_LOOP('',(#3791));
#1127=EDGE_LOOP('',(#3792));
#1128=EDGE_LOOP('',(#3793));
#1129=EDGE_LOOP('',(#3794));
#1130=EDGE_LOOP('',(#3795));
#1131=EDGE_LOOP('',(#3796));
#1132=EDGE_LOOP('',(#3797,#3798,#3799,#3800));
#1133=EDGE_LOOP('',(#3801,#3802));
#1134=EDGE_LOOP('',(#3803));
#1135=EDGE_LOOP('',(#3804));
#1136=EDGE_LOOP('',(#3805));
#1137=EDGE_LOOP('',(#3806));
#1138=EDGE_LOOP('',(#3807));
#1139=EDGE_LOOP('',(#3808));
#1140=EDGE_LOOP('',(#3809,#3810,#3811,#3812));
#1141=EDGE_LOOP('',(#3813,#3814));
#1142=EDGE_LOOP('',(#3815));
#1143=EDGE_LOOP('',(#3816));
#1144=EDGE_LOOP('',(#3817));
#1145=EDGE_LOOP('',(#3818));
#1146=EDGE_LOOP('',(#3819));
#1147=EDGE_LOOP('',(#3820));
#1148=EDGE_LOOP('',(#3821,#3822,#3823,#3824));
#1149=EDGE_LOOP('',(#3825,#3826));
#1150=EDGE_LOOP('',(#3827));
#1151=EDGE_LOOP('',(#3828));
#1152=EDGE_LOOP('',(#3829));
#1153=EDGE_LOOP('',(#3830));
#1154=EDGE_LOOP('',(#3831));
#1155=EDGE_LOOP('',(#3832));
#1156=EDGE_LOOP('',(#3833,#3834,#3835,#3836));
#1157=EDGE_LOOP('',(#3837,#3838));
#1158=EDGE_LOOP('',(#3839));
#1159=EDGE_LOOP('',(#3840));
#1160=EDGE_LOOP('',(#3841));
#1161=EDGE_LOOP('',(#3842));
#1162=EDGE_LOOP('',(#3843));
#1163=EDGE_LOOP('',(#3844));
#1164=EDGE_LOOP('',(#3845,#3846,#3847,#3848));
#1165=EDGE_LOOP('',(#3849,#3850));
#1166=EDGE_LOOP('',(#3851));
#1167=EDGE_LOOP('',(#3852));
#1168=EDGE_LOOP('',(#3853));
#1169=EDGE_LOOP('',(#3854));
#1170=EDGE_LOOP('',(#3855));
#1171=EDGE_LOOP('',(#3856));
#1172=EDGE_LOOP('',(#3857,#3858,#3859,#3860));
#1173=EDGE_LOOP('',(#3861,#3862,#3863,#3864));
#1174=EDGE_LOOP('',(#3865));
#1175=EDGE_LOOP('',(#3866));
#1176=EDGE_LOOP('',(#3867));
#1177=EDGE_LOOP('',(#3868));
#1178=EDGE_LOOP('',(#3869,#3870,#3871,#3872));
#1179=EDGE_LOOP('',(#3873,#3874));
#1180=EDGE_LOOP('',(#3875));
#1181=EDGE_LOOP('',(#3876));
#1182=EDGE_LOOP('',(#3877));
#1183=EDGE_LOOP('',(#3878));
#1184=EDGE_LOOP('',(#3879));
#1185=EDGE_LOOP('',(#3880));
#1186=EDGE_LOOP('',(#3881,#3882,#3883,#3884));
#1187=EDGE_LOOP('',(#3885,#3886));
#1188=EDGE_LOOP('',(#3887));
#1189=EDGE_LOOP('',(#3888));
#1190=EDGE_LOOP('',(#3889));
#1191=EDGE_LOOP('',(#3890));
#1192=EDGE_LOOP('',(#3891));
#1193=EDGE_LOOP('',(#3892));
#1194=EDGE_LOOP('',(#3893,#3894));
#1195=EDGE_LOOP('',(#3895,#3896));
#1196=EDGE_LOOP('',(#3897,#3898,#3899,#3900,#3901));
#1197=EDGE_LOOP('',(#3902,#3903,#3904,#3905,#3906));
#1198=EDGE_LOOP('',(#3907,#3908,#3909,#3910,#3911,#3912));
#1199=EDGE_LOOP('',(#3913,#3914,#3915,#3916,#3917));
#1200=EDGE_LOOP('',(#3918,#3919,#3920,#3921));
#1201=EDGE_LOOP('',(#3922,#3923,#3924,#3925,#3926));
#1202=EDGE_LOOP('',(#3927));
#1203=EDGE_LOOP('',(#3928));
#1204=EDGE_LOOP('',(#3929));
#1205=EDGE_LOOP('',(#3930));
#1206=EDGE_LOOP('',(#3931,#3932,#3933,#3934));
#1207=EDGE_LOOP('',(#3935,#3936,#3937,#3938));
#1208=EDGE_LOOP('',(#3939,#3940,#3941,#3942,#3943));
#1209=EDGE_LOOP('',(#3944,#3945,#3946,#3947,#3948));
#1210=EDGE_LOOP('',(#3949,#3950,#3951,#3952));
#1211=EDGE_LOOP('',(#3953,#3954,#3955,#3956));
#1212=EDGE_LOOP('',(#3957));
#1213=EDGE_LOOP('',(#3958));
#1214=EDGE_LOOP('',(#3959));
#1215=EDGE_LOOP('',(#3960));
#1216=EDGE_LOOP('',(#3961,#3962,#3963,#3964));
#1217=EDGE_LOOP('',(#3965,#3966,#3967,#3968));
#1218=EDGE_LOOP('',(#3969));
#1219=EDGE_LOOP('',(#3970,#3971,#3972,#3973,#3974,#3975));
#1220=EDGE_LOOP('',(#3976,#3977,#3978,#3979));
#1221=EDGE_LOOP('',(#3980,#3981,#3982));
#1222=EDGE_LOOP('',(#3983,#3984,#3985));
#1223=EDGE_LOOP('',(#3986,#3987,#3988));
#1224=EDGE_LOOP('',(#3989,#3990,#3991));
#1225=EDGE_LOOP('',(#3992,#3993,#3994));
#1226=EDGE_LOOP('',(#3995,#3996,#3997));
#1227=EDGE_LOOP('',(#3998,#3999,#4000,#4001));
#1228=EDGE_LOOP('',(#4002,#4003,#4004,#4005));
#1229=EDGE_LOOP('',(#4006,#4007,#4008,#4009));
#1230=EDGE_LOOP('',(#4010,#4011,#4012,#4013));
#1231=EDGE_LOOP('',(#4014,#4015,#4016,#4017));
#1232=EDGE_LOOP('',(#4018,#4019,#4020,#4021));
#1233=EDGE_LOOP('',(#4022,#4023,#4024,#4025));
#1234=EDGE_LOOP('',(#4026));
#1235=EDGE_LOOP('',(#4027));
#1236=EDGE_LOOP('',(#4028));
#1237=EDGE_LOOP('',(#4029,#4030,#4031,#4032));
#1238=EDGE_LOOP('',(#4033));
#1239=EDGE_LOOP('',(#4034,#4035,#4036,#4037));
#1240=EDGE_LOOP('',(#4038));
#1241=EDGE_LOOP('',(#4039));
#1242=EDGE_LOOP('',(#4040));
#1243=EDGE_LOOP('',(#4041,#4042,#4043,#4044));
#1244=EDGE_LOOP('',(#4045));
#1245=EDGE_LOOP('',(#4046));
#1246=EDGE_LOOP('',(#4047));
#1247=EDGE_LOOP('',(#4048,#4049,#4050,#4051));
#1248=EDGE_LOOP('',(#4052));
#1249=EDGE_LOOP('',(#4053,#4054,#4055,#4056));
#1250=EDGE_LOOP('',(#4057));
#1251=EDGE_LOOP('',(#4058,#4059,#4060,#4061));
#1252=EDGE_LOOP('',(#4062));
#1253=EDGE_LOOP('',(#4063));
#1254=EDGE_LOOP('',(#4064));
#1255=EDGE_LOOP('',(#4065,#4066,#4067,#4068));
#1256=EDGE_LOOP('',(#4069));
#1257=EDGE_LOOP('',(#4070));
#1258=EDGE_LOOP('',(#4071,#4072,#4073,#4074));
#1259=EDGE_LOOP('',(#4075,#4076,#4077,#4078));
#1260=EDGE_LOOP('',(#4079,#4080,#4081,#4082,#4083));
#1261=EDGE_LOOP('',(#4084,#4085,#4086,#4087,#4088));
#1262=EDGE_LOOP('',(#4089,#4090,#4091,#4092));
#1263=EDGE_LOOP('',(#4093,#4094,#4095,#4096));
#1264=EDGE_LOOP('',(#4097));
#1265=EDGE_LOOP('',(#4098));
#1266=EDGE_LOOP('',(#4099));
#1267=EDGE_LOOP('',(#4100));
#1268=EDGE_LOOP('',(#4101,#4102));
#1269=EDGE_LOOP('',(#4103,#4104,#4105,#4106));
#1270=EDGE_LOOP('',(#4107,#4108,#4109,#4110));
#1271=EDGE_LOOP('',(#4111,#4112,#4113,#4114));
#1272=EDGE_LOOP('',(#4115,#4116,#4117,#4118));
#1273=EDGE_LOOP('',(#4119,#4120,#4121,#4122,#4123));
#1274=EDGE_LOOP('',(#4124,#4125,#4126,#4127,#4128));
#1275=EDGE_LOOP('',(#4129));
#1276=EDGE_LOOP('',(#4130));
#1277=EDGE_LOOP('',(#4131));
#1278=EDGE_LOOP('',(#4132));
#1279=EDGE_LOOP('',(#4133,#4134));
#1280=EDGE_LOOP('',(#4135,#4136));
#1281=EDGE_LOOP('',(#4137,#4138));
#1282=EDGE_LOOP('',(#4139,#4140));
#1283=EDGE_LOOP('',(#4141,#4142));
#1284=EDGE_LOOP('',(#4143,#4144));
#1285=EDGE_LOOP('',(#4145,#4146));
#1286=EDGE_LOOP('',(#4147,#4148,#4149,#4150));
#1287=EDGE_LOOP('',(#4151,#4152));
#1288=EDGE_LOOP('',(#4153));
#1289=EDGE_LOOP('',(#4154));
#1290=EDGE_LOOP('',(#4155));
#1291=EDGE_LOOP('',(#4156));
#1292=EDGE_LOOP('',(#4157));
#1293=EDGE_LOOP('',(#4158));
#1294=EDGE_LOOP('',(#4159,#4160,#4161,#4162));
#1295=EDGE_LOOP('',(#4163,#4164));
#1296=EDGE_LOOP('',(#4165));
#1297=EDGE_LOOP('',(#4166));
#1298=EDGE_LOOP('',(#4167));
#1299=EDGE_LOOP('',(#4168));
#1300=EDGE_LOOP('',(#4169));
#1301=EDGE_LOOP('',(#4170));
#1302=EDGE_LOOP('',(#4171,#4172,#4173,#4174));
#1303=EDGE_LOOP('',(#4175,#4176));
#1304=EDGE_LOOP('',(#4177));
#1305=EDGE_LOOP('',(#4178));
#1306=EDGE_LOOP('',(#4179));
#1307=EDGE_LOOP('',(#4180));
#1308=EDGE_LOOP('',(#4181));
#1309=EDGE_LOOP('',(#4182));
#1310=EDGE_LOOP('',(#4183,#4184,#4185,#4186));
#1311=EDGE_LOOP('',(#4187,#4188));
#1312=EDGE_LOOP('',(#4189));
#1313=EDGE_LOOP('',(#4190));
#1314=EDGE_LOOP('',(#4191));
#1315=EDGE_LOOP('',(#4192));
#1316=EDGE_LOOP('',(#4193));
#1317=EDGE_LOOP('',(#4194));
#1318=EDGE_LOOP('',(#4195,#4196,#4197,#4198));
#1319=EDGE_LOOP('',(#4199,#4200));
#1320=EDGE_LOOP('',(#4201));
#1321=EDGE_LOOP('',(#4202));
#1322=EDGE_LOOP('',(#4203));
#1323=EDGE_LOOP('',(#4204));
#1324=EDGE_LOOP('',(#4205));
#1325=EDGE_LOOP('',(#4206));
#1326=EDGE_LOOP('',(#4207,#4208,#4209,#4210));
#1327=EDGE_LOOP('',(#4211,#4212));
#1328=EDGE_LOOP('',(#4213));
#1329=EDGE_LOOP('',(#4214));
#1330=EDGE_LOOP('',(#4215));
#1331=EDGE_LOOP('',(#4216));
#1332=EDGE_LOOP('',(#4217));
#1333=EDGE_LOOP('',(#4218));
#1334=EDGE_LOOP('',(#4219,#4220,#4221,#4222));
#1335=EDGE_LOOP('',(#4223,#4224));
#1336=EDGE_LOOP('',(#4225));
#1337=EDGE_LOOP('',(#4226));
#1338=EDGE_LOOP('',(#4227));
#1339=EDGE_LOOP('',(#4228));
#1340=EDGE_LOOP('',(#4229));
#1341=EDGE_LOOP('',(#4230));
#1342=EDGE_LOOP('',(#4231,#4232,#4233,#4234));
#1343=EDGE_LOOP('',(#4235,#4236));
#1344=EDGE_LOOP('',(#4237));
#1345=EDGE_LOOP('',(#4238));
#1346=EDGE_LOOP('',(#4239));
#1347=EDGE_LOOP('',(#4240));
#1348=EDGE_LOOP('',(#4241));
#1349=EDGE_LOOP('',(#4242));
#1350=EDGE_LOOP('',(#4243,#4244,#4245,#4246));
#1351=EDGE_LOOP('',(#4247,#4248,#4249,#4250));
#1352=EDGE_LOOP('',(#4251));
#1353=EDGE_LOOP('',(#4252));
#1354=EDGE_LOOP('',(#4253));
#1355=EDGE_LOOP('',(#4254));
#1356=EDGE_LOOP('',(#4255,#4256,#4257,#4258,#4259));
#1357=EDGE_LOOP('',(#4260,#4261,#4262,#4263,#4264));
#1358=EDGE_LOOP('',(#4265,#4266,#4267,#4268,#4269,#4270));
#1359=EDGE_LOOP('',(#4271,#4272,#4273,#4274,#4275));
#1360=EDGE_LOOP('',(#4276,#4277,#4278,#4279));
#1361=EDGE_LOOP('',(#4280,#4281,#4282,#4283,#4284));
#1362=EDGE_LOOP('',(#4285));
#1363=EDGE_LOOP('',(#4286));
#1364=EDGE_LOOP('',(#4287));
#1365=EDGE_LOOP('',(#4288));
#1366=EDGE_LOOP('',(#4289,#4290,#4291,#4292));
#1367=EDGE_LOOP('',(#4293,#4294,#4295,#4296));
#1368=EDGE_LOOP('',(#4297,#4298,#4299,#4300,#4301));
#1369=EDGE_LOOP('',(#4302,#4303,#4304,#4305,#4306));
#1370=EDGE_LOOP('',(#4307,#4308,#4309,#4310));
#1371=EDGE_LOOP('',(#4311,#4312,#4313,#4314));
#1372=EDGE_LOOP('',(#4315));
#1373=EDGE_LOOP('',(#4316));
#1374=EDGE_LOOP('',(#4317));
#1375=EDGE_LOOP('',(#4318));
#1376=EDGE_LOOP('',(#4319,#4320,#4321,#4322,#4323));
#1377=EDGE_LOOP('',(#4324,#4325,#4326,#4327,#4328));
#1378=EDGE_LOOP('',(#4329,#4330,#4331,#4332,#4333));
#1379=EDGE_LOOP('',(#4334,#4335,#4336,#4337,#4338));
#1380=EDGE_LOOP('',(#4339,#4340,#4341,#4342,#4343));
#1381=EDGE_LOOP('',(#4344,#4345,#4346,#4347,#4348));
#1382=EDGE_LOOP('',(#4349,#4350,#4351,#4352,#4353));
#1383=EDGE_LOOP('',(#4354,#4355,#4356,#4357,#4358));
#1384=EDGE_LOOP('',(#4359,#4360,#4361,#4362));
#1385=EDGE_LOOP('',(#4363,#4364,#4365,#4366));
#1386=EDGE_LOOP('',(#4367,#4368,#4369,#4370));
#1387=EDGE_LOOP('',(#4371,#4372,#4373,#4374));
#1388=EDGE_LOOP('',(#4375));
#1389=EDGE_LOOP('',(#4376));
#1390=EDGE_LOOP('',(#4377,#4378,#4379,#4380));
#1391=EDGE_LOOP('',(#4381,#4382,#4383,#4384,#4385,#4386,#4387,#4388,#4389,
#4390,#4391,#4392,#4393,#4394,#4395,#4396,#4397,#4398,#4399,#4400,#4401,
#4402,#4403,#4404));
#1392=EDGE_LOOP('',(#4405));
#1393=EDGE_LOOP('',(#4406));
#1394=EDGE_LOOP('',(#4407));
#1395=EDGE_LOOP('',(#4408,#4409,#4410,#4411));
#1396=EDGE_LOOP('',(#4412,#4413,#4414,#4415));
#1397=EDGE_LOOP('',(#4416,#4417,#4418,#4419));
#1398=EDGE_LOOP('',(#4420,#4421,#4422,#4423,#4424,#4425,#4426,#4427,#4428,
#4429,#4430,#4431,#4432,#4433,#4434,#4435,#4436,#4437,#4438,#4439,#4440,
#4441,#4442,#4443));
#1399=EDGE_LOOP('',(#4444));
#1400=EDGE_LOOP('',(#4445));
#1401=EDGE_LOOP('',(#4446));
#1402=EDGE_LOOP('',(#4447,#4448,#4449,#4450));
#1403=EDGE_LOOP('',(#4451));
#1404=EDGE_LOOP('',(#4452));
#1405=EDGE_LOOP('',(#4453,#4454,#4455,#4456));
#1406=EDGE_LOOP('',(#4457,#4458,#4459,#4460));
#1407=EDGE_LOOP('',(#4461,#4462,#4463,#4464));
#1408=EDGE_LOOP('',(#4465,#4466,#4467,#4468));
#1409=EDGE_LOOP('',(#4469));
#1410=EDGE_LOOP('',(#4470));
#1411=EDGE_LOOP('',(#4471,#4472,#4473,#4474));
#1412=EDGE_LOOP('',(#4475,#4476,#4477,#4478));
#1413=EDGE_LOOP('',(#4479,#4480,#4481,#4482));
#1414=EDGE_LOOP('',(#4483,#4484,#4485,#4486));
#1415=EDGE_LOOP('',(#4487,#4488,#4489,#4490));
#1416=EDGE_LOOP('',(#4491));
#1417=EDGE_LOOP('',(#4492));
#1418=EDGE_LOOP('',(#4493,#4494,#4495,#4496));
#1419=EDGE_LOOP('',(#4497,#4498));
#1420=EDGE_LOOP('',(#4499,#4500));
#1421=EDGE_LOOP('',(#4501,#4502));
#1422=EDGE_LOOP('',(#4503,#4504));
#1423=EDGE_LOOP('',(#4505,#4506,#4507,#4508));
#1424=EDGE_LOOP('',(#4509,#4510));
#1425=EDGE_LOOP('',(#4511,#4512));
#1426=EDGE_LOOP('',(#4513,#4514));
#1427=EDGE_LOOP('',(#4515,#4516));
#1428=EDGE_LOOP('',(#4517,#4518,#4519,#4520));
#1429=EDGE_LOOP('',(#4521,#4522,#4523,#4524));
#1430=EDGE_LOOP('',(#4525,#4526,#4527,#4528));
#1431=EDGE_LOOP('',(#4529,#4530,#4531,#4532));
#1432=EDGE_LOOP('',(#4533,#4534,#4535,#4536));
#1433=EDGE_LOOP('',(#4537,#4538,#4539,#4540));
#1434=EDGE_LOOP('',(#4541,#4542,#4543,#4544));
#1435=LINE('',#7477,#1672);
#1436=LINE('',#7486,#1673);
#1437=LINE('',#7493,#1674);
#1438=LINE('',#7500,#1675);
#1439=LINE('',#7507,#1676);
#1440=LINE('',#7513,#1677);
#1441=LINE('',#7518,#1678);
#1442=LINE('',#7523,#1679);
#1443=LINE('',#7527,#1680);
#1444=LINE('',#7531,#1681);
#1445=LINE('',#7533,#1682);
#1446=LINE('',#7535,#1683);
#1447=LINE('',#7537,#1684);
#1448=LINE('',#7539,#1685);
#1449=LINE('',#7541,#1686);
#1450=LINE('',#7542,#1687);
#1451=LINE('',#7545,#1688);
#1452=LINE('',#7547,#1689);
#1453=LINE('',#7549,#1690);
#1454=LINE('',#7553,#1691);
#1455=LINE('',#7557,#1692);
#1456=LINE('',#7563,#1693);
#1457=LINE('',#7567,#1694);
#1458=LINE('',#7568,#1695);
#1459=LINE('',#7571,#1696);
#1460=LINE('',#7575,#1697);
#1461=LINE('',#7576,#1698);
#1462=LINE('',#7579,#1699);
#1463=LINE('',#7583,#1700);
#1464=LINE('',#7586,#1701);
#1465=LINE('',#7599,#1702);
#1466=LINE('',#7600,#1703);
#1467=LINE('',#7613,#1704);
#1468=LINE('',#7615,#1705);
#1469=LINE('',#7624,#1706);
#1470=LINE('',#7626,#1707);
#1471=LINE('',#7627,#1708);
#1472=LINE('',#7634,#1709);
#1473=LINE('',#7637,#1710);
#1474=LINE('',#7639,#1711);
#1475=LINE('',#7641,#1712);
#1476=LINE('',#7643,#1713);
#1477=LINE('',#7644,#1714);
#1478=LINE('',#7646,#1715);
#1479=LINE('',#7647,#1716);
#1480=LINE('',#7649,#1717);
#1481=LINE('',#7661,#1718);
#1482=LINE('',#7668,#1719);
#1483=LINE('',#7677,#1720);
#1484=LINE('',#7684,#1721);
#1485=LINE('',#7691,#1722);
#1486=LINE('',#7700,#1723);
#1487=LINE('',#7706,#1724);
#1488=LINE('',#7709,#1725);
#1489=LINE('',#7740,#1726);
#1490=LINE('',#7741,#1727);
#1491=LINE('',#7757,#1728);
#1492=LINE('',#7758,#1729);
#1493=LINE('',#7767,#1730);
#1494=LINE('',#7768,#1731);
#1495=LINE('',#7770,#1732);
#1496=LINE('',#7771,#1733);
#1497=LINE('',#7780,#1734);
#1498=LINE('',#7781,#1735);
#1499=LINE('',#7783,#1736);
#1500=LINE('',#7784,#1737);
#1501=LINE('',#7786,#1738);
#1502=LINE('',#7787,#1739);
#1503=LINE('',#7789,#1740);
#1504=LINE('',#7790,#1741);
#1505=LINE('',#7792,#1742);
#1506=LINE('',#7793,#1743);
#1507=LINE('',#7795,#1744);
#1508=LINE('',#7796,#1745);
#1509=LINE('',#7798,#1746);
#1510=LINE('',#7799,#1747);
#1511=LINE('',#7801,#1748);
#1512=LINE('',#7802,#1749);
#1513=LINE('',#7815,#1750);
#1514=LINE('',#7820,#1751);
#1515=LINE('',#7834,#1752);
#1516=LINE('',#7838,#1753);
#1517=LINE('',#7844,#1754);
#1518=LINE('',#7849,#1755);
#1519=LINE('',#7852,#1756);
#1520=LINE('',#7864,#1757);
#1521=LINE('',#7870,#1758);
#1522=LINE('',#7879,#1759);
#1523=LINE('',#7886,#1760);
#1524=LINE('',#7889,#1761);
#1525=LINE('',#8352,#1762);
#1526=LINE('',#8358,#1763);
#1527=LINE('',#8475,#1764);
#1528=LINE('',#8479,#1765);
#1529=LINE('',#8484,#1766);
#1530=LINE('',#8487,#1767);
#1531=LINE('',#8507,#1768);
#1532=LINE('',#8511,#1769);
#1533=LINE('',#8516,#1770);
#1534=LINE('',#8519,#1771);
#1535=LINE('',#8527,#1772);
#1536=LINE('',#8538,#1773);
#1537=LINE('',#8540,#1774);
#1538=LINE('',#8542,#1775);
#1539=LINE('',#8544,#1776);
#1540=LINE('',#8546,#1777);
#1541=LINE('',#8547,#1778);
#1542=LINE('',#8551,#1779);
#1543=LINE('',#8555,#1780);
#1544=LINE('',#8557,#1781);
#1545=LINE('',#8558,#1782);
#1546=LINE('',#8561,#1783);
#1547=LINE('',#8562,#1784);
#1548=LINE('',#8565,#1785);
#1549=LINE('',#8566,#1786);
#1550=LINE('',#8569,#1787);
#1551=LINE('',#8570,#1788);
#1552=LINE('',#8573,#1789);
#1553=LINE('',#8574,#1790);
#1554=LINE('',#8576,#1791);
#1555=LINE('',#8578,#1792);
#1556=LINE('',#8579,#1793);
#1557=LINE('',#8581,#1794);
#1558=LINE('',#8583,#1795);
#1559=LINE('',#8585,#1796);
#1560=LINE('',#8587,#1797);
#1561=LINE('',#8591,#1798);
#1562=LINE('',#8600,#1799);
#1563=LINE('',#8607,#1800);
#1564=LINE('',#8615,#1801);
#1565=LINE('',#8625,#1802);
#1566=LINE('',#8632,#1803);
#1567=LINE('',#8639,#1804);
#1568=LINE('',#8648,#1805);
#1569=LINE('',#8661,#1806);
#1570=LINE('',#8668,#1807);
#1571=LINE('',#8671,#1808);
#1572=LINE('',#8675,#1809);
#1573=LINE('',#8680,#1810);
#1574=LINE('',#8691,#1811);
#1575=LINE('',#8697,#1812);
#1576=LINE('',#8705,#1813);
#1577=LINE('',#8712,#1814);
#1578=LINE('',#8716,#1815);
#1579=LINE('',#8879,#1816);
#1580=LINE('',#8885,#1817);
#1581=LINE('',#8907,#1818);
#1582=LINE('',#8914,#1819);
#1583=LINE('',#8919,#1820);
#1584=LINE('',#8922,#1821);
#1585=LINE('',#8939,#1822);
#1586=LINE('',#8946,#1823);
#1587=LINE('',#8951,#1824);
#1588=LINE('',#8954,#1825);
#1589=LINE('',#8962,#1826);
#1590=LINE('',#9040,#1827);
#1591=LINE('',#9046,#1828);
#1592=LINE('',#9124,#1829);
#1593=LINE('',#9130,#1830);
#1594=LINE('',#9208,#1831);
#1595=LINE('',#9214,#1832);
#1596=LINE('',#9292,#1833);
#1597=LINE('',#9297,#1834);
#1598=LINE('',#9299,#1835);
#1599=LINE('',#9301,#1836);
#1600=LINE('',#9302,#1837);
#1601=LINE('',#9305,#1838);
#1602=LINE('',#9307,#1839);
#1603=LINE('',#9308,#1840);
#1604=LINE('',#9311,#1841);
#1605=LINE('',#9313,#1842);
#1606=LINE('',#9314,#1843);
#1607=LINE('',#9317,#1844);
#1608=LINE('',#9319,#1845);
#1609=LINE('',#9320,#1846);
#1610=LINE('',#9323,#1847);
#1611=LINE('',#9325,#1848);
#1612=LINE('',#9326,#1849);
#1613=LINE('',#9329,#1850);
#1614=LINE('',#9331,#1851);
#1615=LINE('',#9333,#1852);
#1616=LINE('',#9335,#1853);
#1617=LINE('',#9337,#1854);
#1618=LINE('',#9339,#1855);
#1619=LINE('',#9341,#1856);
#1620=LINE('',#9343,#1857);
#1621=LINE('',#9345,#1858);
#1622=LINE('',#9347,#1859);
#1623=LINE('',#9349,#1860);
#1624=LINE('',#9351,#1861);
#1625=LINE('',#9353,#1862);
#1626=LINE('',#9355,#1863);
#1627=LINE('',#9357,#1864);
#1628=LINE('',#9359,#1865);
#1629=LINE('',#9361,#1866);
#1630=LINE('',#9363,#1867);
#1631=LINE('',#9364,#1868);
#1632=LINE('',#9373,#1869);
#1633=LINE('',#9375,#1870);
#1634=LINE('',#9376,#1871);
#1635=LINE('',#9379,#1872);
#1636=LINE('',#9380,#1873);
#1637=LINE('',#9382,#1874);
#1638=LINE('',#9385,#1875);
#1639=LINE('',#9387,#1876);
#1640=LINE('',#9389,#1877);
#1641=LINE('',#9391,#1878);
#1642=LINE('',#9393,#1879);
#1643=LINE('',#9395,#1880);
#1644=LINE('',#9397,#1881);
#1645=LINE('',#9399,#1882);
#1646=LINE('',#9401,#1883);
#1647=LINE('',#9403,#1884);
#1648=LINE('',#9405,#1885);
#1649=LINE('',#9407,#1886);
#1650=LINE('',#9409,#1887);
#1651=LINE('',#9411,#1888);
#1652=LINE('',#9413,#1889);
#1653=LINE('',#9414,#1890);
#1654=LINE('',#9422,#1891);
#1655=LINE('',#9424,#1892);
#1656=LINE('',#9425,#1893);
#1657=LINE('',#9427,#1894);
#1658=LINE('',#9429,#1895);
#1659=LINE('',#9431,#1896);
#1660=LINE('',#9433,#1897);
#1661=LINE('',#9435,#1898);
#1662=LINE('',#9436,#1899);
#1663=LINE('',#9438,#1900);
#1664=LINE('',#9441,#1901);
#1665=LINE('',#9443,#1902);
#1666=LINE('',#9445,#1903);
#1667=LINE('',#9447,#1904);
#1668=LINE('',#9449,#1905);
#1669=LINE('',#9451,#1906);
#1670=LINE('',#9454,#1907);
#1671=LINE('',#9456,#1908);
#1672=VECTOR('',#5834,6.00000000000001);
#1673=VECTOR('',#5845,4.);
#1674=VECTOR('',#5854,4.);
#1675=VECTOR('',#5863,5.);
#1676=VECTOR('',#5872,3.00000000000001);
#1677=VECTOR('',#5879,3.00000000000001);
#1678=VECTOR('',#5886,4.99999999999977);
#1679=VECTOR('',#5891,10.);
#1680=VECTOR('',#5894,10.);
#1681=VECTOR('',#5899,10.);
#1682=VECTOR('',#5900,10.);
#1683=VECTOR('',#5901,10.);
#1684=VECTOR('',#5902,10.);
#1685=VECTOR('',#5903,10.);
#1686=VECTOR('',#5904,10.);
#1687=VECTOR('',#5905,10.);
#1688=VECTOR('',#5908,10.);
#1689=VECTOR('',#5909,10.);
#1690=VECTOR('',#5910,10.);
#1691=VECTOR('',#5913,10.);
#1692=VECTOR('',#5918,10.);
#1693=VECTOR('',#5925,10.);
#1694=VECTOR('',#5928,10.);
#1695=VECTOR('',#5929,10.);
#1696=VECTOR('',#5932,10.);
#1697=VECTOR('',#5937,10.);
#1698=VECTOR('',#5938,10.);
#1699=VECTOR('',#5941,10.);
#1700=VECTOR('',#5946,10.);
#1701=VECTOR('',#5949,10.);
#1702=VECTOR('',#5966,10.);
#1703=VECTOR('',#5967,10.);
#1704=VECTOR('',#5984,10.);
#1705=VECTOR('',#5985,10.);
#1706=VECTOR('',#5998,10.);
#1707=VECTOR('',#6001,10.);
#1708=VECTOR('',#6002,10.);
#1709=VECTOR('',#6011,10.);
#1710=VECTOR('',#6016,10.);
#1711=VECTOR('',#6019,10.);
#1712=VECTOR('',#6022,10.);
#1713=VECTOR('',#6025,10.);
#1714=VECTOR('',#6026,10.);
#1715=VECTOR('',#6029,10.);
#1716=VECTOR('',#6030,10.);
#1717=VECTOR('',#6033,10.);
#1718=VECTOR('',#6052,7.50000000000001);
#1719=VECTOR('',#6061,6.00000000000001);
#1720=VECTOR('',#6072,4.);
#1721=VECTOR('',#6081,4.);
#1722=VECTOR('',#6090,4.99999999999977);
#1723=VECTOR('',#6101,4.99999999999977);
#1724=VECTOR('',#6110,3.);
#1725=VECTOR('',#6113,3.);
#1726=VECTOR('',#6150,10.);
#1727=VECTOR('',#6151,10.);
#1728=VECTOR('',#6170,10.);
#1729=VECTOR('',#6171,10.);
#1730=VECTOR('',#6182,10.);
#1731=VECTOR('',#6183,10.);
#1732=VECTOR('',#6186,10.);
#1733=VECTOR('',#6187,10.);
#1734=VECTOR('',#6198,10.);
#1735=VECTOR('',#6199,10.);
#1736=VECTOR('',#6202,10.);
#1737=VECTOR('',#6203,10.);
#1738=VECTOR('',#6206,10.);
#1739=VECTOR('',#6207,10.);
#1740=VECTOR('',#6210,10.);
#1741=VECTOR('',#6211,10.);
#1742=VECTOR('',#6214,10.);
#1743=VECTOR('',#6215,10.);
#1744=VECTOR('',#6218,10.);
#1745=VECTOR('',#6219,10.);
#1746=VECTOR('',#6222,10.);
#1747=VECTOR('',#6223,10.);
#1748=VECTOR('',#6226,10.);
#1749=VECTOR('',#6227,10.);
#1750=VECTOR('',#6246,6.00000000000001);
#1751=VECTOR('',#6253,7.50000000000001);
#1752=VECTOR('',#6272,6.24999999999999);
#1753=VECTOR('',#6277,6.);
#1754=VECTOR('',#6284,6.);
#1755=VECTOR('',#6291,7.24999999999999);
#1756=VECTOR('',#6294,7.24999999999999);
#1757=VECTOR('',#6309,10.25);
#1758=VECTOR('',#6316,9.25000000000001);
#1759=VECTOR('',#6329,9.25);
#1760=VECTOR('',#6336,10.5);
#1761=VECTOR('',#6341,10.5);
#1762=VECTOR('',#6566,8.25);
#1763=VECTOR('',#6573,8.75);
#1764=VECTOR('',#6650,9.1);
#1765=VECTOR('',#6655,9.25000000000001);
#1766=VECTOR('',#6660,7.39999999999999);
#1767=VECTOR('',#6665,7.39999999999999);
#1768=VECTOR('',#6692,7.39999999999999);
#1769=VECTOR('',#6697,7.24999999999999);
#1770=VECTOR('',#6702,9.1);
#1771=VECTOR('',#6707,9.1);
#1772=VECTOR('',#6718,2.72327499999996);
#1773=VECTOR('',#6731,10.);
#1774=VECTOR('',#6732,10.);
#1775=VECTOR('',#6733,10.);
#1776=VECTOR('',#6734,10.);
#1777=VECTOR('',#6735,9.99999999999999);
#1778=VECTOR('',#6736,10.);
#1779=VECTOR('',#6741,4.99999999999977);
#1780=VECTOR('',#6744,9.99999999999999);
#1781=VECTOR('',#6745,10.);
#1782=VECTOR('',#6746,10.);
#1783=VECTOR('',#6749,10.);
#1784=VECTOR('',#6750,10.);
#1785=VECTOR('',#6753,9.99999999999999);
#1786=VECTOR('',#6754,9.99999999999999);
#1787=VECTOR('',#6757,10.);
#1788=VECTOR('',#6758,10.);
#1789=VECTOR('',#6761,10.);
#1790=VECTOR('',#6762,10.);
#1791=VECTOR('',#6765,10.);
#1792=VECTOR('',#6768,10.);
#1793=VECTOR('',#6769,10.);
#1794=VECTOR('',#6772,10.);
#1795=VECTOR('',#6775,10.);
#1796=VECTOR('',#6778,10.);
#1797=VECTOR('',#6781,10.);
#1798=VECTOR('',#6786,2.942);
#1799=VECTOR('',#6799,3.);
#1800=VECTOR('',#6808,3.);
#1801=VECTOR('',#6819,6.00000000000001);
#1802=VECTOR('',#6834,7.50000000000001);
#1803=VECTOR('',#6843,3.);
#1804=VECTOR('',#6852,3.);
#1805=VECTOR('',#6865,6.00000000000001);
#1806=VECTOR('',#6882,8.04999999999999);
#1807=VECTOR('',#6891,7.5);
#1808=VECTOR('',#6894,7.5);
#1809=VECTOR('',#6899,11.);
#1810=VECTOR('',#6906,11.);
#1811=VECTOR('',#6919,16.95);
#1812=VECTOR('',#6926,14.);
#1813=VECTOR('',#6937,14.);
#1814=VECTOR('',#6944,17.5);
#1815=VECTOR('',#6951,17.5);
#1816=VECTOR('',#7148,12.5);
#1817=VECTOR('',#7155,13.25);
#1818=VECTOR('',#7184,13.775);
#1819=VECTOR('',#7193,14.);
#1820=VECTOR('',#7198,11.225);
#1821=VECTOR('',#7203,11.225);
#1822=VECTOR('',#7226,11.225);
#1823=VECTOR('',#7235,11.);
#1824=VECTOR('',#7240,13.775);
#1825=VECTOR('',#7245,13.775);
#1826=VECTOR('',#7256,2.5);
#1827=VECTOR('',#7259,2.5);
#1828=VECTOR('',#7266,2.5);
#1829=VECTOR('',#7269,2.5);
#1830=VECTOR('',#7276,2.5);
#1831=VECTOR('',#7279,2.5);
#1832=VECTOR('',#7286,2.5);
#1833=VECTOR('',#7289,2.5);
#1834=VECTOR('',#7294,10.);
#1835=VECTOR('',#7295,10.);
#1836=VECTOR('',#7296,10.);
#1837=VECTOR('',#7297,10.);
#1838=VECTOR('',#7300,10.);
#1839=VECTOR('',#7301,10.);
#1840=VECTOR('',#7302,10.);
#1841=VECTOR('',#7305,10.);
#1842=VECTOR('',#7306,10.);
#1843=VECTOR('',#7307,10.);
#1844=VECTOR('',#7310,10.);
#1845=VECTOR('',#7311,10.);
#1846=VECTOR('',#7312,10.);
#1847=VECTOR('',#7315,10.);
#1848=VECTOR('',#7316,10.);
#1849=VECTOR('',#7317,10.);
#1850=VECTOR('',#7320,10.);
#1851=VECTOR('',#7321,10.);
#1852=VECTOR('',#7322,10.);
#1853=VECTOR('',#7323,10.);
#1854=VECTOR('',#7324,10.);
#1855=VECTOR('',#7325,10.);
#1856=VECTOR('',#7326,10.);
#1857=VECTOR('',#7327,10.);
#1858=VECTOR('',#7328,10.);
#1859=VECTOR('',#7329,10.);
#1860=VECTOR('',#7330,10.);
#1861=VECTOR('',#7331,10.);
#1862=VECTOR('',#7332,10.);
#1863=VECTOR('',#7333,10.);
#1864=VECTOR('',#7334,10.);
#1865=VECTOR('',#7335,10.);
#1866=VECTOR('',#7336,10.);
#1867=VECTOR('',#7337,10.);
#1868=VECTOR('',#7338,10.);
#1869=VECTOR('',#7347,10.);
#1870=VECTOR('',#7348,10.);
#1871=VECTOR('',#7349,10.);
#1872=VECTOR('',#7352,10.);
#1873=VECTOR('',#7353,10.);
#1874=VECTOR('',#7356,10.);
#1875=VECTOR('',#7359,10.);
#1876=VECTOR('',#7360,10.);
#1877=VECTOR('',#7361,10.);
#1878=VECTOR('',#7362,10.);
#1879=VECTOR('',#7363,10.);
#1880=VECTOR('',#7364,10.);
#1881=VECTOR('',#7365,10.);
#1882=VECTOR('',#7366,10.);
#1883=VECTOR('',#7367,10.);
#1884=VECTOR('',#7368,10.);
#1885=VECTOR('',#7369,10.);
#1886=VECTOR('',#7370,10.);
#1887=VECTOR('',#7371,10.);
#1888=VECTOR('',#7372,10.);
#1889=VECTOR('',#7373,10.);
#1890=VECTOR('',#7374,10.);
#1891=VECTOR('',#7383,10.);
#1892=VECTOR('',#7386,10.);
#1893=VECTOR('',#7387,10.);
#1894=VECTOR('',#7390,10.);
#1895=VECTOR('',#7393,10.);
#1896=VECTOR('',#7396,10.);
#1897=VECTOR('',#7399,10.);
#1898=VECTOR('',#7402,10.);
#1899=VECTOR('',#7403,10.);
#1900=VECTOR('',#7406,10.);
#1901=VECTOR('',#7411,10.);
#1902=VECTOR('',#7414,10.5);
#1903=VECTOR('',#7417,10.5);
#1904=VECTOR('',#7420,17.5);
#1905=VECTOR('',#7423,10.);
#1906=VECTOR('',#7426,10.);
#1907=VECTOR('',#7431,10.);
#1908=VECTOR('',#7434,10.);
#1909=CIRCLE('',#5125,6.00000000000001);
#1910=CIRCLE('',#5126,6.00000000000001);
#1911=CIRCLE('',#5128,4.99999999999977);
#1912=CIRCLE('',#5130,4.);
#1913=CIRCLE('',#5131,4.);
#1914=CIRCLE('',#5134,4.);
#1915=CIRCLE('',#5135,4.);
#1916=CIRCLE('',#5138,5.);
#1917=CIRCLE('',#5139,5.);
#1918=CIRCLE('',#5141,3.00000000000001);
#1919=CIRCLE('',#5143,3.00000000000001);
#1920=CIRCLE('',#5145,3.00000000000001);
#1921=CIRCLE('',#5146,3.00000000000001);
#1922=CIRCLE('',#5149,4.99999999999977);
#1923=CIRCLE('',#5151,4.99999999999977);
#1924=CIRCLE('',#5152,4.99999999999977);
#1925=CIRCLE('',#5155,1.);
#1926=CIRCLE('',#5156,1.);
#1927=CIRCLE('',#5158,6.00000000000001);
#1928=CIRCLE('',#5160,1.);
#1929=CIRCLE('',#5161,1.);
#1930=CIRCLE('',#5163,1.);
#1931=CIRCLE('',#5166,0.999999999999996);
#1932=CIRCLE('',#5168,1.);
#1933=CIRCLE('',#5170,0.999999999999996);
#1934=CIRCLE('',#5171,0.999999999999996);
#1935=CIRCLE('',#5172,1.);
#1936=CIRCLE('',#5174,0.999999999999996);
#1937=CIRCLE('',#5175,0.999999999999996);
#1938=CIRCLE('',#5178,0.999999999999996);
#1939=CIRCLE('',#5179,0.999999999999996);
#1940=CIRCLE('',#5180,1.);
#1941=CIRCLE('',#5182,0.999999999999996);
#1942=CIRCLE('',#5183,1.);
#1943=CIRCLE('',#5187,0.999999999999996);
#1944=CIRCLE('',#5188,0.999999999999996);
#1945=CIRCLE('',#5189,1.);
#1946=CIRCLE('',#5193,0.999999999999996);
#1947=CIRCLE('',#5194,0.999999999999996);
#1948=CIRCLE('',#5204,6.00000000000001);
#1949=CIRCLE('',#5205,7.50000000000001);
#1950=CIRCLE('',#5210,7.50000000000001);
#1951=CIRCLE('',#5215,6.00000000000001);
#1952=CIRCLE('',#5216,6.00000000000001);
#1953=CIRCLE('',#5218,3.);
#1954=CIRCLE('',#5220,4.);
#1955=CIRCLE('',#5221,4.);
#1956=CIRCLE('',#5224,4.);
#1957=CIRCLE('',#5225,4.);
#1958=CIRCLE('',#5228,4.99999999999977);
#1959=CIRCLE('',#5229,4.99999999999977);
#1960=CIRCLE('',#5231,3.);
#1961=CIRCLE('',#5233,4.99999999999977);
#1962=CIRCLE('',#5234,4.99999999999977);
#1963=CIRCLE('',#5236,3.);
#1964=CIRCLE('',#5239,3.);
#1965=CIRCLE('',#5241,0.999999999999996);
#1966=CIRCLE('',#5242,0.999999999999996);
#1967=CIRCLE('',#5243,1.);
#1968=CIRCLE('',#5245,0.999999999999996);
#1969=CIRCLE('',#5246,1.00000000000001);
#1970=CIRCLE('',#5247,1.);
#1971=CIRCLE('',#5249,0.999999999999996);
#1972=CIRCLE('',#5250,1.00000000000001);
#1973=CIRCLE('',#5251,1.);
#1974=CIRCLE('',#5253,0.999999999999996);
#1975=CIRCLE('',#5254,0.999999999999996);
#1976=CIRCLE('',#5255,1.);
#1977=CIRCLE('',#5258,0.999999999999996);
#1978=CIRCLE('',#5259,0.999999999999996);
#1979=CIRCLE('',#5260,1.);
#1980=CIRCLE('',#5262,0.999999999999996);
#1981=CIRCLE('',#5263,0.999999999999996);
#1982=CIRCLE('',#5264,1.);
#1983=CIRCLE('',#5267,0.999999999999996);
#1984=CIRCLE('',#5268,0.999999999999996);
#1985=CIRCLE('',#5269,1.);
#1986=CIRCLE('',#5273,0.999999999999996);
#1987=CIRCLE('',#5274,1.00000000000001);
#1988=CIRCLE('',#5275,1.);
#1989=CIRCLE('',#5285,7.50000000000001);
#1990=CIRCLE('',#5286,6.00000000000001);
#1991=CIRCLE('',#5293,6.00000000000001);
#1992=CIRCLE('',#5296,7.50000000000001);
#1993=CIRCLE('',#5300,7.24999999999999);
#1994=CIRCLE('',#5301,1.49484711634153);
#1995=CIRCLE('',#5302,7.24999999999999);
#1996=CIRCLE('',#5304,6.);
#1997=CIRCLE('',#5305,6.24999999999999);
#1998=CIRCLE('',#5307,6.);
#1999=CIRCLE('',#5308,6.);
#2000=CIRCLE('',#5310,6.24999999999999);
#2001=CIRCLE('',#5312,7.24999999999999);
#2002=CIRCLE('',#5314,7.24999999999999);
#2003=CIRCLE('',#5318,1.49484711634153);
#2004=CIRCLE('',#5320,10.5);
#2005=CIRCLE('',#5321,10.25);
#2006=CIRCLE('',#5323,9.25000000000001);
#2007=CIRCLE('',#5324,9.25);
#2008=CIRCLE('',#5326,1.49484711634153);
#2009=CIRCLE('',#5327,9.25);
#2010=CIRCLE('',#5329,9.25000000000001);
#2011=CIRCLE('',#5331,10.5);
#2012=CIRCLE('',#5332,10.5);
#2013=CIRCLE('',#5333,10.25);
#2014=CIRCLE('',#5338,1.49484711634153);
#2015=CIRCLE('',#5340,1.49484711634153);
#2016=CIRCLE('',#5342,1.49484711634153);
#2017=CIRCLE('',#5344,1.49484711634153);
#2018=CIRCLE('',#5346,1.49484711634153);
#2019=CIRCLE('',#5348,1.49484711634153);
#2020=CIRCLE('',#5350,1.49484711634153);
#2021=CIRCLE('',#5352,1.49484711634153);
#2022=CIRCLE('',#5354,1.49484711634153);
#2023=CIRCLE('',#5355,1.59062243825056);
#2024=CIRCLE('',#5356,1.42003545260829);
#2025=CIRCLE('',#5357,1.59062243825056);
#2026=CIRCLE('',#5359,1.49484711634152);
#2027=CIRCLE('',#5360,1.40874692590067);
#2028=CIRCLE('',#5361,1.40874692590067);
#2029=CIRCLE('',#5364,1.59062243825056);
#2030=CIRCLE('',#5365,1.42003545260833);
#2031=CIRCLE('',#5366,1.59062243825056);
#2032=CIRCLE('',#5368,1.49484711634152);
#2033=CIRCLE('',#5369,1.40874692590067);
#2034=CIRCLE('',#5370,1.40874692590067);
#2035=CIRCLE('',#5373,1.59062243825056);
#2036=CIRCLE('',#5374,1.42003545260828);
#2037=CIRCLE('',#5375,1.59062243825056);
#2038=CIRCLE('',#5377,1.49484711634152);
#2039=CIRCLE('',#5378,1.40874692590067);
#2040=CIRCLE('',#5379,1.40874692590067);
#2041=CIRCLE('',#5382,1.59062243825056);
#2042=CIRCLE('',#5383,1.4200354526083);
#2043=CIRCLE('',#5384,1.59062243825056);
#2044=CIRCLE('',#5386,1.49484711634152);
#2045=CIRCLE('',#5387,1.40874692590067);
#2046=CIRCLE('',#5388,1.40874692590067);
#2047=CIRCLE('',#5391,1.59062243825056);
#2048=CIRCLE('',#5392,1.42003545260827);
#2049=CIRCLE('',#5393,1.59062243825056);
#2050=CIRCLE('',#5395,1.49484711634152);
#2051=CIRCLE('',#5396,1.40874692590067);
#2052=CIRCLE('',#5397,1.40874692590067);
#2053=CIRCLE('',#5400,1.59062243825056);
#2054=CIRCLE('',#5401,1.42003545260833);
#2055=CIRCLE('',#5402,1.59062243825056);
#2056=CIRCLE('',#5404,1.49484711634152);
#2057=CIRCLE('',#5405,1.40874692590067);
#2058=CIRCLE('',#5406,1.40874692590067);
#2059=CIRCLE('',#5409,1.59062243825056);
#2060=CIRCLE('',#5410,1.42003545260831);
#2061=CIRCLE('',#5411,1.59062243825056);
#2062=CIRCLE('',#5413,1.49484711634152);
#2063=CIRCLE('',#5414,1.40874692590067);
#2064=CIRCLE('',#5415,1.40874692590067);
#2065=CIRCLE('',#5418,1.59062243825056);
#2066=CIRCLE('',#5419,1.42003545260829);
#2067=CIRCLE('',#5420,1.59062243825056);
#2068=CIRCLE('',#5422,1.49484711634152);
#2069=CIRCLE('',#5423,1.40874692590067);
#2070=CIRCLE('',#5424,1.40874692590067);
#2071=CIRCLE('',#5427,1.59062243825056);
#2072=CIRCLE('',#5428,1.42003545260828);
#2073=CIRCLE('',#5429,1.59062243825056);
#2074=CIRCLE('',#5431,1.49484711634152);
#2075=CIRCLE('',#5432,1.40874692590067);
#2076=CIRCLE('',#5433,1.40874692590067);
#2077=CIRCLE('',#5436,1.59062243825056);
#2078=CIRCLE('',#5437,1.42003545260832);
#2079=CIRCLE('',#5438,1.59062243825056);
#2080=CIRCLE('',#5440,1.49484711634152);
#2081=CIRCLE('',#5441,1.40874692590067);
#2082=CIRCLE('',#5442,1.40874692590067);
#2083=CIRCLE('',#5446,8.25);
#2084=CIRCLE('',#5447,8.25);
#2085=CIRCLE('',#5449,8.75);
#2086=CIRCLE('',#5450,8.75);
#2087=CIRCLE('',#5453,1.59062243825056);
#2088=CIRCLE('',#5454,1.42003545260827);
#2089=CIRCLE('',#5455,1.59062243825056);
#2090=CIRCLE('',#5457,1.49484711634152);
#2091=CIRCLE('',#5458,1.40874692590067);
#2092=CIRCLE('',#5459,1.40874692590067);
#2093=CIRCLE('',#5462,1.59062243825056);
#2094=CIRCLE('',#5463,1.42003545260827);
#2095=CIRCLE('',#5464,1.59062243825056);
#2096=CIRCLE('',#5466,1.49484711634152);
#2097=CIRCLE('',#5467,1.40874692590067);
#2098=CIRCLE('',#5468,1.40874692590067);
#2099=CIRCLE('',#5472,1.49484711634153);
#2100=CIRCLE('',#5474,1.49484711634153);
#2101=CIRCLE('',#5476,7.42777777777777);
#2102=CIRCLE('',#5477,0.0277777777777778);
#2103=CIRCLE('',#5478,7.39999999999999);
#2104=CIRCLE('',#5479,7.39999999999999);
#2105=CIRCLE('',#5481,9.1);
#2106=CIRCLE('',#5482,0.0277777777777778);
#2107=CIRCLE('',#5483,9.07222222222223);
#2108=CIRCLE('',#5484,9.1);
#2109=CIRCLE('',#5486,9.1);
#2110=CIRCLE('',#5487,9.1);
#2111=CIRCLE('',#5489,9.25000000000001);
#2112=CIRCLE('',#5491,7.24999999999999);
#2113=CIRCLE('',#5492,7.39999999999999);
#2114=CIRCLE('',#5497,9.1);
#2115=CIRCLE('',#5498,0.027777777777778);
#2116=CIRCLE('',#5499,9.07222222222222);
#2117=CIRCLE('',#5501,7.42777777777777);
#2118=CIRCLE('',#5502,0.027777777777778);
#2119=CIRCLE('',#5503,7.39999999999999);
#2120=CIRCLE('',#5505,7.39999999999999);
#2121=CIRCLE('',#5506,7.39999999999999);
#2122=CIRCLE('',#5508,7.24999999999999);
#2123=CIRCLE('',#5510,9.25);
#2124=CIRCLE('',#5511,9.1);
#2125=CIRCLE('',#5517,2.942);
#2126=CIRCLE('',#5518,2.38654999999999);
#2127=CIRCLE('',#5520,4.99999999999977);
#2128=CIRCLE('',#5521,0.6);
#2129=CIRCLE('',#5522,4.39999999999977);
#2130=CIRCLE('',#5525,4.99999999999977);
#2131=CIRCLE('',#5539,2.942);
#2132=CIRCLE('',#5544,3.);
#2133=CIRCLE('',#5545,3.);
#2134=CIRCLE('',#5548,3.);
#2135=CIRCLE('',#5549,3.);
#2136=CIRCLE('',#5552,6.00000000000001);
#2137=CIRCLE('',#5554,6.00000000000001);
#2138=CIRCLE('',#5558,7.50000000000001);
#2139=CIRCLE('',#5560,7.50000000000001);
#2140=CIRCLE('',#5564,3.);
#2141=CIRCLE('',#5565,3.);
#2142=CIRCLE('',#5568,3.);
#2143=CIRCLE('',#5569,3.);
#2144=CIRCLE('',#5572,6.00000000000001);
#2145=CIRCLE('',#5574,6.00000000000001);
#2146=CIRCLE('',#5578,11.);
#2147=CIRCLE('',#5579,2.86797988869785);
#2148=CIRCLE('',#5580,11.);
#2149=CIRCLE('',#5582,7.5);
#2150=CIRCLE('',#5583,8.04999999999999);
#2151=CIRCLE('',#5585,7.5);
#2152=CIRCLE('',#5586,7.5);
#2153=CIRCLE('',#5588,8.04999999999999);
#2154=CIRCLE('',#5590,11.);
#2155=CIRCLE('',#5592,11.);
#2156=CIRCLE('',#5596,2.86797988869785);
#2157=CIRCLE('',#5598,17.5);
#2158=CIRCLE('',#5599,16.95);
#2159=CIRCLE('',#5601,14.);
#2160=CIRCLE('',#5602,14.);
#2161=CIRCLE('',#5604,2.86797988869785);
#2162=CIRCLE('',#5605,14.);
#2163=CIRCLE('',#5607,14.);
#2164=CIRCLE('',#5609,17.5);
#2165=CIRCLE('',#5610,16.95);
#2166=CIRCLE('',#5611,17.5);
#2167=CIRCLE('',#5616,2.86797988869785);
#2168=CIRCLE('',#5618,2.86797988869785);
#2169=CIRCLE('',#5620,2.86797988869785);
#2170=CIRCLE('',#5622,2.86797988869785);
#2171=CIRCLE('',#5624,2.86797988869785);
#2172=CIRCLE('',#5626,2.86797988869785);
#2173=CIRCLE('',#5628,2.86797988869785);
#2174=CIRCLE('',#5630,3.22348154659542);
#2175=CIRCLE('',#5631,1.34926506255229);
#2176=CIRCLE('',#5632,3.22348154659542);
#2177=CIRCLE('',#5634,2.86797988869795);
#2178=CIRCLE('',#5635,2.7681778559145);
#2179=CIRCLE('',#5636,2.7681778559145);
#2180=CIRCLE('',#5640,3.22348154659542);
#2181=CIRCLE('',#5641,1.34926506255229);
#2182=CIRCLE('',#5642,3.22348154659542);
#2183=CIRCLE('',#5644,2.86797988869795);
#2184=CIRCLE('',#5645,2.7681778559145);
#2185=CIRCLE('',#5646,2.7681778559145);
#2186=CIRCLE('',#5650,3.22348154659542);
#2187=CIRCLE('',#5651,1.34926506255229);
#2188=CIRCLE('',#5652,3.22348154659542);
#2189=CIRCLE('',#5654,2.86797988869795);
#2190=CIRCLE('',#5655,2.7681778559145);
#2191=CIRCLE('',#5656,2.7681778559145);
#2192=CIRCLE('',#5660,3.22348154659542);
#2193=CIRCLE('',#5661,1.34926506255229);
#2194=CIRCLE('',#5662,3.22348154659542);
#2195=CIRCLE('',#5664,2.86797988869795);
#2196=CIRCLE('',#5665,2.7681778559145);
#2197=CIRCLE('',#5666,2.7681778559145);
#2198=CIRCLE('',#5670,3.22348154659542);
#2199=CIRCLE('',#5671,1.34926506255229);
#2200=CIRCLE('',#5672,3.22348154659542);
#2201=CIRCLE('',#5674,2.86797988869795);
#2202=CIRCLE('',#5675,2.7681778559145);
#2203=CIRCLE('',#5676,2.7681778559145);
#2204=CIRCLE('',#5680,3.22348154659542);
#2205=CIRCLE('',#5681,1.34926506255229);
#2206=CIRCLE('',#5682,3.22348154659542);
#2207=CIRCLE('',#5684,2.86797988869795);
#2208=CIRCLE('',#5685,2.7681778559145);
#2209=CIRCLE('',#5686,2.7681778559145);
#2210=CIRCLE('',#5690,3.22348154659542);
#2211=CIRCLE('',#5691,1.34926506255229);
#2212=CIRCLE('',#5692,3.22348154659542);
#2213=CIRCLE('',#5694,2.86797988869795);
#2214=CIRCLE('',#5695,2.7681778559145);
#2215=CIRCLE('',#5696,2.7681778559145);
#2216=CIRCLE('',#5700,3.22348154659542);
#2217=CIRCLE('',#5701,1.34926506255229);
#2218=CIRCLE('',#5702,3.22348154659542);
#2219=CIRCLE('',#5704,2.86797988869795);
#2220=CIRCLE('',#5705,2.7681778559145);
#2221=CIRCLE('',#5706,2.7681778559145);
#2222=CIRCLE('',#5710,12.5);
#2223=CIRCLE('',#5711,12.5);
#2224=CIRCLE('',#5713,13.25);
#2225=CIRCLE('',#5714,13.25);
#2226=CIRCLE('',#5718,11.2861111111111);
#2227=CIRCLE('',#5719,0.0611111111111111);
#2228=CIRCLE('',#5720,11.225);
#2229=CIRCLE('',#5721,11.225);
#2230=CIRCLE('',#5723,13.775);
#2231=CIRCLE('',#5724,13.775);
#2232=CIRCLE('',#5725,0.0611111111111111);
#2233=CIRCLE('',#5726,13.7138888888889);
#2234=CIRCLE('',#5728,13.775);
#2235=CIRCLE('',#5729,13.775);
#2236=CIRCLE('',#5731,14.);
#2237=CIRCLE('',#5733,11.);
#2238=CIRCLE('',#5734,11.225);
#2239=CIRCLE('',#5739,13.775);
#2240=CIRCLE('',#5740,0.061111111111111);
#2241=CIRCLE('',#5741,13.7138888888889);
#2242=CIRCLE('',#5743,11.2861111111111);
#2243=CIRCLE('',#5744,0.061111111111111);
#2244=CIRCLE('',#5745,11.225);
#2245=CIRCLE('',#5747,11.225);
#2246=CIRCLE('',#5748,11.225);
#2247=CIRCLE('',#5750,11.);
#2248=CIRCLE('',#5752,14.);
#2249=CIRCLE('',#5753,13.775);
#2250=CIRCLE('',#5759,2.5);
#2251=CIRCLE('',#5761,2.5);
#2252=CIRCLE('',#5763,2.5);
#2253=CIRCLE('',#5765,2.5);
#2254=CIRCLE('',#5767,2.5);
#2255=CIRCLE('',#5769,2.5);
#2256=CIRCLE('',#5771,2.5);
#2257=CIRCLE('',#5773,2.5);
#2258=CIRCLE('',#5780,10.5);
#2259=CIRCLE('',#5781,10.5);
#2260=CIRCLE('',#5782,17.5);
#2261=CIRCLE('',#5787,10.5);
#2262=CIRCLE('',#5788,10.5);
#2263=CIRCLE('',#5789,17.5);
#2264=VERTEX_POINT('',#7474);
#2265=VERTEX_POINT('',#7476);
#2266=VERTEX_POINT('',#7480);
#2267=VERTEX_POINT('',#7483);
#2268=VERTEX_POINT('',#7485);
#2269=VERTEX_POINT('',#7490);
#2270=VERTEX_POINT('',#7492);
#2271=VERTEX_POINT('',#7497);
#2272=VERTEX_POINT('',#7499);
#2273=VERTEX_POINT('',#7503);
#2274=VERTEX_POINT('',#7506);
#2275=VERTEX_POINT('',#7510);
#2276=VERTEX_POINT('',#7512);
#2277=VERTEX_POINT('',#7517);
#2278=VERTEX_POINT('',#7521);
#2279=VERTEX_POINT('',#7522);
#2280=VERTEX_POINT('',#7524);
#2281=VERTEX_POINT('',#7526);
#2282=VERTEX_POINT('',#7530);
#2283=VERTEX_POINT('',#7532);
#2284=VERTEX_POINT('',#7534);
#2285=VERTEX_POINT('',#7536);
#2286=VERTEX_POINT('',#7538);
#2287=VERTEX_POINT('',#7540);
#2288=VERTEX_POINT('',#7544);
#2289=VERTEX_POINT('',#7546);
#2290=VERTEX_POINT('',#7548);
#2291=VERTEX_POINT('',#7550);
#2292=VERTEX_POINT('',#7552);
#2293=VERTEX_POINT('',#7556);
#2294=VERTEX_POINT('',#7560);
#2295=VERTEX_POINT('',#7562);
#2296=VERTEX_POINT('',#7564);
#2297=VERTEX_POINT('',#7566);
#2298=VERTEX_POINT('',#7570);
#2299=VERTEX_POINT('',#7574);
#2300=VERTEX_POINT('',#7578);
#2301=VERTEX_POINT('',#7582);
#2302=VERTEX_POINT('',#7584);
#2303=VERTEX_POINT('',#7588);
#2304=VERTEX_POINT('',#7589);
#2305=VERTEX_POINT('',#7591);
#2306=VERTEX_POINT('',#7595);
#2307=VERTEX_POINT('',#7602);
#2308=VERTEX_POINT('',#7603);
#2309=VERTEX_POINT('',#7608);
#2310=VERTEX_POINT('',#7612);
#2311=VERTEX_POINT('',#7614);
#2312=VERTEX_POINT('',#7618);
#2313=VERTEX_POINT('',#7620);
#2314=VERTEX_POINT('',#7629);
#2315=VERTEX_POINT('',#7633);
#2316=VERTEX_POINT('',#7652);
#2317=VERTEX_POINT('',#7658);
#2318=VERTEX_POINT('',#7665);
#2319=VERTEX_POINT('',#7667);
#2320=VERTEX_POINT('',#7671);
#2321=VERTEX_POINT('',#7674);
#2322=VERTEX_POINT('',#7676);
#2323=VERTEX_POINT('',#7681);
#2324=VERTEX_POINT('',#7683);
#2325=VERTEX_POINT('',#7688);
#2326=VERTEX_POINT('',#7690);
#2327=VERTEX_POINT('',#7694);
#2328=VERTEX_POINT('',#7697);
#2329=VERTEX_POINT('',#7699);
#2330=VERTEX_POINT('',#7703);
#2331=VERTEX_POINT('',#7708);
#2332=VERTEX_POINT('',#7712);
#2333=VERTEX_POINT('',#7713);
#2334=VERTEX_POINT('',#7715);
#2335=VERTEX_POINT('',#7719);
#2336=VERTEX_POINT('',#7720);
#2337=VERTEX_POINT('',#7722);
#2338=VERTEX_POINT('',#7726);
#2339=VERTEX_POINT('',#7727);
#2340=VERTEX_POINT('',#7729);
#2341=VERTEX_POINT('',#7733);
#2342=VERTEX_POINT('',#7734);
#2343=VERTEX_POINT('',#7736);
#2344=VERTEX_POINT('',#7743);
#2345=VERTEX_POINT('',#7744);
#2346=VERTEX_POINT('',#7746);
#2347=VERTEX_POINT('',#7750);
#2348=VERTEX_POINT('',#7751);
#2349=VERTEX_POINT('',#7753);
#2350=VERTEX_POINT('',#7760);
#2351=VERTEX_POINT('',#7761);
#2352=VERTEX_POINT('',#7763);
#2353=VERTEX_POINT('',#7773);
#2354=VERTEX_POINT('',#7774);
#2355=VERTEX_POINT('',#7776);
#2356=VERTEX_POINT('',#7804);
#2357=VERTEX_POINT('',#7806);
#2358=VERTEX_POINT('',#7814);
#2359=VERTEX_POINT('',#7819);
#2360=VERTEX_POINT('',#7825);
#2361=VERTEX_POINT('',#7827);
#2362=VERTEX_POINT('',#7831);
#2363=VERTEX_POINT('',#7833);
#2364=VERTEX_POINT('',#7837);
#2365=VERTEX_POINT('',#7839);
#2366=VERTEX_POINT('',#7843);
#2367=VERTEX_POINT('',#7847);
#2368=VERTEX_POINT('',#7851);
#2369=VERTEX_POINT('',#7857);
#2370=VERTEX_POINT('',#7858);
#2371=VERTEX_POINT('',#7861);
#2372=VERTEX_POINT('',#7863);
#2373=VERTEX_POINT('',#7867);
#2374=VERTEX_POINT('',#7869);
#2375=VERTEX_POINT('',#7873);
#2376=VERTEX_POINT('',#7877);
#2377=VERTEX_POINT('',#7881);
#2378=VERTEX_POINT('',#7882);
#2379=VERTEX_POINT('',#7885);
#2380=VERTEX_POINT('',#7893);
#2381=VERTEX_POINT('',#7894);
#2382=VERTEX_POINT('',#7897);
#2383=VERTEX_POINT('',#7898);
#2384=VERTEX_POINT('',#7901);
#2385=VERTEX_POINT('',#7902);
#2386=VERTEX_POINT('',#7905);
#2387=VERTEX_POINT('',#7906);
#2388=VERTEX_POINT('',#7909);
#2389=VERTEX_POINT('',#7910);
#2390=VERTEX_POINT('',#7913);
#2391=VERTEX_POINT('',#7914);
#2392=VERTEX_POINT('',#7917);
#2393=VERTEX_POINT('',#7918);
#2394=VERTEX_POINT('',#7921);
#2395=VERTEX_POINT('',#7922);
#2396=VERTEX_POINT('',#7925);
#2397=VERTEX_POINT('',#7926);
#2398=VERTEX_POINT('',#7955);
#2399=VERTEX_POINT('',#7957);
#2400=VERTEX_POINT('',#7961);
#2401=VERTEX_POINT('',#7962);
#2402=VERTEX_POINT('',#7964);
#2403=VERTEX_POINT('',#7966);
#2404=VERTEX_POINT('',#7997);
#2405=VERTEX_POINT('',#7999);
#2406=VERTEX_POINT('',#8003);
#2407=VERTEX_POINT('',#8004);
#2408=VERTEX_POINT('',#8006);
#2409=VERTEX_POINT('',#8008);
#2410=VERTEX_POINT('',#8039);
#2411=VERTEX_POINT('',#8041);
#2412=VERTEX_POINT('',#8045);
#2413=VERTEX_POINT('',#8046);
#2414=VERTEX_POINT('',#8048);
#2415=VERTEX_POINT('',#8050);
#2416=VERTEX_POINT('',#8081);
#2417=VERTEX_POINT('',#8083);
#2418=VERTEX_POINT('',#8087);
#2419=VERTEX_POINT('',#8088);
#2420=VERTEX_POINT('',#8090);
#2421=VERTEX_POINT('',#8092);
#2422=VERTEX_POINT('',#8123);
#2423=VERTEX_POINT('',#8125);
#2424=VERTEX_POINT('',#8129);
#2425=VERTEX_POINT('',#8130);
#2426=VERTEX_POINT('',#8132);
#2427=VERTEX_POINT('',#8134);
#2428=VERTEX_POINT('',#8165);
#2429=VERTEX_POINT('',#8167);
#2430=VERTEX_POINT('',#8171);
#2431=VERTEX_POINT('',#8172);
#2432=VERTEX_POINT('',#8174);
#2433=VERTEX_POINT('',#8176);
#2434=VERTEX_POINT('',#8207);
#2435=VERTEX_POINT('',#8209);
#2436=VERTEX_POINT('',#8213);
#2437=VERTEX_POINT('',#8214);
#2438=VERTEX_POINT('',#8216);
#2439=VERTEX_POINT('',#8218);
#2440=VERTEX_POINT('',#8249);
#2441=VERTEX_POINT('',#8251);
#2442=VERTEX_POINT('',#8255);
#2443=VERTEX_POINT('',#8256);
#2444=VERTEX_POINT('',#8258);
#2445=VERTEX_POINT('',#8260);
#2446=VERTEX_POINT('',#8291);
#2447=VERTEX_POINT('',#8293);
#2448=VERTEX_POINT('',#8297);
#2449=VERTEX_POINT('',#8298);
#2450=VERTEX_POINT('',#8300);
#2451=VERTEX_POINT('',#8302);
#2452=VERTEX_POINT('',#8333);
#2453=VERTEX_POINT('',#8335);
#2454=VERTEX_POINT('',#8339);
#2455=VERTEX_POINT('',#8340);
#2456=VERTEX_POINT('',#8342);
#2457=VERTEX_POINT('',#8344);
#2458=VERTEX_POINT('',#8349);
#2459=VERTEX_POINT('',#8351);
#2460=VERTEX_POINT('',#8355);
#2461=VERTEX_POINT('',#8357);
#2462=VERTEX_POINT('',#8389);
#2463=VERTEX_POINT('',#8391);
#2464=VERTEX_POINT('',#8395);
#2465=VERTEX_POINT('',#8396);
#2466=VERTEX_POINT('',#8398);
#2467=VERTEX_POINT('',#8400);
#2468=VERTEX_POINT('',#8431);
#2469=VERTEX_POINT('',#8433);
#2470=VERTEX_POINT('',#8437);
#2471=VERTEX_POINT('',#8438);
#2472=VERTEX_POINT('',#8440);
#2473=VERTEX_POINT('',#8442);
#2474=VERTEX_POINT('',#8447);
#2475=VERTEX_POINT('',#8448);
#2476=VERTEX_POINT('',#8451);
#2477=VERTEX_POINT('',#8452);
#2478=VERTEX_POINT('',#8455);
#2479=VERTEX_POINT('',#8457);
#2480=VERTEX_POINT('',#8459);
#2481=VERTEX_POINT('',#8463);
#2482=VERTEX_POINT('',#8464);
#2483=VERTEX_POINT('',#8466);
#2484=VERTEX_POINT('',#8471);
#2485=VERTEX_POINT('',#8472);
#2486=VERTEX_POINT('',#8477);
#2487=VERTEX_POINT('',#8481);
#2488=VERTEX_POINT('',#8483);
#2489=VERTEX_POINT('',#8491);
#2490=VERTEX_POINT('',#8493);
#2491=VERTEX_POINT('',#8497);
#2492=VERTEX_POINT('',#8499);
#2493=VERTEX_POINT('',#8503);
#2494=VERTEX_POINT('',#8504);
#2495=VERTEX_POINT('',#8509);
#2496=VERTEX_POINT('',#8513);
#2497=VERTEX_POINT('',#8515);
#2498=VERTEX_POINT('',#8524);
#2499=VERTEX_POINT('',#8526);
#2500=VERTEX_POINT('',#8530);
#2501=VERTEX_POINT('',#8532);
#2502=VERTEX_POINT('',#8536);
#2503=VERTEX_POINT('',#8537);
#2504=VERTEX_POINT('',#8539);
#2505=VERTEX_POINT('',#8541);
#2506=VERTEX_POINT('',#8543);
#2507=VERTEX_POINT('',#8545);
#2508=VERTEX_POINT('',#8549);
#2509=VERTEX_POINT('',#8553);
#2510=VERTEX_POINT('',#8554);
#2511=VERTEX_POINT('',#8556);
#2512=VERTEX_POINT('',#8560);
#2513=VERTEX_POINT('',#8564);
#2514=VERTEX_POINT('',#8568);
#2515=VERTEX_POINT('',#8572);
#2516=VERTEX_POINT('',#8590);
#2517=VERTEX_POINT('',#8597);
#2518=VERTEX_POINT('',#8599);
#2519=VERTEX_POINT('',#8604);
#2520=VERTEX_POINT('',#8606);
#2521=VERTEX_POINT('',#8611);
#2522=VERTEX_POINT('',#8614);
#2523=VERTEX_POINT('',#8620);
#2524=VERTEX_POINT('',#8623);
#2525=VERTEX_POINT('',#8629);
#2526=VERTEX_POINT('',#8631);
#2527=VERTEX_POINT('',#8636);
#2528=VERTEX_POINT('',#8638);
#2529=VERTEX_POINT('',#8643);
#2530=VERTEX_POINT('',#8646);
#2531=VERTEX_POINT('',#8652);
#2532=VERTEX_POINT('',#8654);
#2533=VERTEX_POINT('',#8658);
#2534=VERTEX_POINT('',#8660);
#2535=VERTEX_POINT('',#8664);
#2536=VERTEX_POINT('',#8665);
#2537=VERTEX_POINT('',#8670);
#2538=VERTEX_POINT('',#8674);
#2539=VERTEX_POINT('',#8678);
#2540=VERTEX_POINT('',#8684);
#2541=VERTEX_POINT('',#8685);
#2542=VERTEX_POINT('',#8688);
#2543=VERTEX_POINT('',#8690);
#2544=VERTEX_POINT('',#8694);
#2545=VERTEX_POINT('',#8696);
#2546=VERTEX_POINT('',#8700);
#2547=VERTEX_POINT('',#8704);
#2548=VERTEX_POINT('',#8708);
#2549=VERTEX_POINT('',#8709);
#2550=VERTEX_POINT('',#8711);
#2551=VERTEX_POINT('',#8720);
#2552=VERTEX_POINT('',#8721);
#2553=VERTEX_POINT('',#8724);
#2554=VERTEX_POINT('',#8725);
#2555=VERTEX_POINT('',#8728);
#2556=VERTEX_POINT('',#8729);
#2557=VERTEX_POINT('',#8732);
#2558=VERTEX_POINT('',#8733);
#2559=VERTEX_POINT('',#8736);
#2560=VERTEX_POINT('',#8737);
#2561=VERTEX_POINT('',#8740);
#2562=VERTEX_POINT('',#8741);
#2563=VERTEX_POINT('',#8744);
#2564=VERTEX_POINT('',#8745);
#2565=VERTEX_POINT('',#8748);
#2566=VERTEX_POINT('',#8750);
#2567=VERTEX_POINT('',#8754);
#2568=VERTEX_POINT('',#8755);
#2569=VERTEX_POINT('',#8757);
#2570=VERTEX_POINT('',#8759);
#2571=VERTEX_POINT('',#8764);
#2572=VERTEX_POINT('',#8766);
#2573=VERTEX_POINT('',#8770);
#2574=VERTEX_POINT('',#8771);
#2575=VERTEX_POINT('',#8773);
#2576=VERTEX_POINT('',#8775);
#2577=VERTEX_POINT('',#8780);
#2578=VERTEX_POINT('',#8782);
#2579=VERTEX_POINT('',#8786);
#2580=VERTEX_POINT('',#8787);
#2581=VERTEX_POINT('',#8789);
#2582=VERTEX_POINT('',#8791);
#2583=VERTEX_POINT('',#8796);
#2584=VERTEX_POINT('',#8798);
#2585=VERTEX_POINT('',#8802);
#2586=VERTEX_POINT('',#8803);
#2587=VERTEX_POINT('',#8805);
#2588=VERTEX_POINT('',#8807);
#2589=VERTEX_POINT('',#8812);
#2590=VERTEX_POINT('',#8814);
#2591=VERTEX_POINT('',#8818);
#2592=VERTEX_POINT('',#8819);
#2593=VERTEX_POINT('',#8821);
#2594=VERTEX_POINT('',#8823);
#2595=VERTEX_POINT('',#8828);
#2596=VERTEX_POINT('',#8830);
#2597=VERTEX_POINT('',#8834);
#2598=VERTEX_POINT('',#8835);
#2599=VERTEX_POINT('',#8837);
#2600=VERTEX_POINT('',#8839);
#2601=VERTEX_POINT('',#8844);
#2602=VERTEX_POINT('',#8846);
#2603=VERTEX_POINT('',#8850);
#2604=VERTEX_POINT('',#8851);
#2605=VERTEX_POINT('',#8853);
#2606=VERTEX_POINT('',#8855);
#2607=VERTEX_POINT('',#8860);
#2608=VERTEX_POINT('',#8862);
#2609=VERTEX_POINT('',#8866);
#2610=VERTEX_POINT('',#8867);
#2611=VERTEX_POINT('',#8869);
#2612=VERTEX_POINT('',#8871);
#2613=VERTEX_POINT('',#8876);
#2614=VERTEX_POINT('',#8878);
#2615=VERTEX_POINT('',#8882);
#2616=VERTEX_POINT('',#8884);
#2617=VERTEX_POINT('',#8890);
#2618=VERTEX_POINT('',#8892);
#2619=VERTEX_POINT('',#8894);
#2620=VERTEX_POINT('',#8898);
#2621=VERTEX_POINT('',#8899);
#2622=VERTEX_POINT('',#8902);
#2623=VERTEX_POINT('',#8906);
#2624=VERTEX_POINT('',#8908);
#2625=VERTEX_POINT('',#8912);
#2626=VERTEX_POINT('',#8916);
#2627=VERTEX_POINT('',#8918);
#2628=VERTEX_POINT('',#8926);
#2629=VERTEX_POINT('',#8928);
#2630=VERTEX_POINT('',#8932);
#2631=VERTEX_POINT('',#8934);
#2632=VERTEX_POINT('',#8938);
#2633=VERTEX_POINT('',#8940);
#2634=VERTEX_POINT('',#8944);
#2635=VERTEX_POINT('',#8948);
#2636=VERTEX_POINT('',#8950);
#2637=VERTEX_POINT('',#8959);
#2638=VERTEX_POINT('',#8961);
#2639=VERTEX_POINT('',#8963);
#2640=VERTEX_POINT('',#9001);
#2641=VERTEX_POINT('',#9002);
#2642=VERTEX_POINT('',#9039);
#2643=VERTEX_POINT('',#9043);
#2644=VERTEX_POINT('',#9045);
#2645=VERTEX_POINT('',#9047);
#2646=VERTEX_POINT('',#9085);
#2647=VERTEX_POINT('',#9086);
#2648=VERTEX_POINT('',#9123);
#2649=VERTEX_POINT('',#9127);
#2650=VERTEX_POINT('',#9129);
#2651=VERTEX_POINT('',#9131);
#2652=VERTEX_POINT('',#9169);
#2653=VERTEX_POINT('',#9170);
#2654=VERTEX_POINT('',#9207);
#2655=VERTEX_POINT('',#9211);
#2656=VERTEX_POINT('',#9213);
#2657=VERTEX_POINT('',#9215);
#2658=VERTEX_POINT('',#9253);
#2659=VERTEX_POINT('',#9254);
#2660=VERTEX_POINT('',#9291);
#2661=VERTEX_POINT('',#9295);
#2662=VERTEX_POINT('',#9296);
#2663=VERTEX_POINT('',#9298);
#2664=VERTEX_POINT('',#9300);
#2665=VERTEX_POINT('',#9304);
#2666=VERTEX_POINT('',#9306);
#2667=VERTEX_POINT('',#9310);
#2668=VERTEX_POINT('',#9312);
#2669=VERTEX_POINT('',#9316);
#2670=VERTEX_POINT('',#9318);
#2671=VERTEX_POINT('',#9322);
#2672=VERTEX_POINT('',#9324);
#2673=VERTEX_POINT('',#9328);
#2674=VERTEX_POINT('',#9330);
#2675=VERTEX_POINT('',#9332);
#2676=VERTEX_POINT('',#9334);
#2677=VERTEX_POINT('',#9336);
#2678=VERTEX_POINT('',#9338);
#2679=VERTEX_POINT('',#9340);
#2680=VERTEX_POINT('',#9342);
#2681=VERTEX_POINT('',#9344);
#2682=VERTEX_POINT('',#9346);
#2683=VERTEX_POINT('',#9348);
#2684=VERTEX_POINT('',#9350);
#2685=VERTEX_POINT('',#9352);
#2686=VERTEX_POINT('',#9354);
#2687=VERTEX_POINT('',#9356);
#2688=VERTEX_POINT('',#9358);
#2689=VERTEX_POINT('',#9360);
#2690=VERTEX_POINT('',#9362);
#2691=VERTEX_POINT('',#9365);
#2692=VERTEX_POINT('',#9367);
#2693=VERTEX_POINT('',#9369);
#2694=VERTEX_POINT('',#9372);
#2695=VERTEX_POINT('',#9374);
#2696=VERTEX_POINT('',#9378);
#2697=VERTEX_POINT('',#9384);
#2698=VERTEX_POINT('',#9386);
#2699=VERTEX_POINT('',#9388);
#2700=VERTEX_POINT('',#9390);
#2701=VERTEX_POINT('',#9392);
#2702=VERTEX_POINT('',#9394);
#2703=VERTEX_POINT('',#9396);
#2704=VERTEX_POINT('',#9398);
#2705=VERTEX_POINT('',#9400);
#2706=VERTEX_POINT('',#9402);
#2707=VERTEX_POINT('',#9404);
#2708=VERTEX_POINT('',#9406);
#2709=VERTEX_POINT('',#9408);
#2710=VERTEX_POINT('',#9410);
#2711=VERTEX_POINT('',#9412);
#2712=VERTEX_POINT('',#9415);
#2713=VERTEX_POINT('',#9417);
#2714=VERTEX_POINT('',#9419);
#2715=EDGE_CURVE('',#2264,#2264,#1909,.T.);
#2716=EDGE_CURVE('',#2264,#2265,#1435,.T.);
#2717=EDGE_CURVE('',#2265,#2265,#1910,.T.);
#2718=EDGE_CURVE('',#2266,#2266,#1911,.T.);
#2719=EDGE_CURVE('',#2267,#2267,#1912,.T.);
#2720=EDGE_CURVE('',#2267,#2268,#1436,.T.);
#2721=EDGE_CURVE('',#2268,#2268,#1913,.T.);
#2722=EDGE_CURVE('',#2269,#2269,#1914,.T.);
#2723=EDGE_CURVE('',#2269,#2270,#1437,.T.);
#2724=EDGE_CURVE('',#2270,#2270,#1915,.T.);
#2725=EDGE_CURVE('',#2271,#2271,#1916,.T.);
#2726=EDGE_CURVE('',#2271,#2272,#1438,.T.);
#2727=EDGE_CURVE('',#2272,#2272,#1917,.T.);
#2728=EDGE_CURVE('',#2273,#2273,#1918,.T.);
#2729=EDGE_CURVE('',#2273,#2274,#1439,.T.);
#2730=EDGE_CURVE('',#2274,#2274,#1919,.T.);
#2731=EDGE_CURVE('',#2275,#2275,#1920,.T.);
#2732=EDGE_CURVE('',#2275,#2276,#1440,.T.);
#2733=EDGE_CURVE('',#2276,#2276,#1921,.T.);
#2734=EDGE_CURVE('',#2266,#2277,#1441,.T.);
#2735=EDGE_CURVE('',#2277,#2277,#1922,.T.);
#2736=EDGE_CURVE('',#2278,#2279,#1442,.T.);
#2737=EDGE_CURVE('',#2280,#2278,#1923,.T.);
#2738=EDGE_CURVE('',#2281,#2280,#1443,.T.);
#2739=EDGE_CURVE('',#2279,#2281,#1924,.T.);
#2740=EDGE_CURVE('',#2281,#2282,#1444,.T.);
#2741=EDGE_CURVE('',#2283,#2282,#1445,.T.);
#2742=EDGE_CURVE('',#2284,#2283,#1446,.T.);
#2743=EDGE_CURVE('',#2285,#2284,#1447,.T.);
#2744=EDGE_CURVE('',#2286,#2285,#1448,.T.);
#2745=EDGE_CURVE('',#2287,#2286,#1449,.T.);
#2746=EDGE_CURVE('',#2287,#2279,#1450,.T.);
#2747=EDGE_CURVE('',#2288,#2280,#1451,.T.);
#2748=EDGE_CURVE('',#2289,#2288,#1452,.T.);
#2749=EDGE_CURVE('',#2290,#2289,#1453,.T.);
#2750=EDGE_CURVE('',#2291,#2290,#1925,.T.);
#2751=EDGE_CURVE('',#2292,#2291,#1454,.T.);
#2752=EDGE_CURVE('',#2282,#2292,#1926,.T.);
#2753=EDGE_CURVE('',#2278,#2293,#1455,.T.);
#2754=EDGE_CURVE('',#2288,#2293,#1927,.T.);
#2755=EDGE_CURVE('',#2294,#2287,#1928,.T.);
#2756=EDGE_CURVE('',#2295,#2294,#1456,.T.);
#2757=EDGE_CURVE('',#2296,#2295,#1929,.T.);
#2758=EDGE_CURVE('',#2297,#2296,#1457,.T.);
#2759=EDGE_CURVE('',#2293,#2297,#1458,.T.);
#2760=EDGE_CURVE('',#2292,#2298,#1459,.T.);
#2761=EDGE_CURVE('',#2298,#2283,#1930,.F.);
#2762=EDGE_CURVE('',#2299,#2291,#1460,.T.);
#2763=EDGE_CURVE('',#2298,#2299,#1461,.T.);
#2764=EDGE_CURVE('',#2290,#2300,#1462,.T.);
#2765=EDGE_CURVE('',#2300,#2299,#1931,.F.);
#2766=EDGE_CURVE('',#2295,#2301,#1463,.T.);
#2767=EDGE_CURVE('',#2301,#2302,#1932,.F.);
#2768=EDGE_CURVE('',#2302,#2296,#1464,.T.);
#2769=EDGE_CURVE('',#2303,#2304,#1933,.F.);
#2770=EDGE_CURVE('',#2305,#2303,#1934,.F.);
#2771=EDGE_CURVE('',#2304,#2305,#1935,.F.);
#2772=EDGE_CURVE('',#2306,#2301,#1936,.F.);
#2773=EDGE_CURVE('',#2302,#2306,#1937,.F.);
#2774=EDGE_CURVE('',#2306,#2305,#1465,.T.);
#2775=EDGE_CURVE('',#2303,#2302,#1466,.T.);
#2776=EDGE_CURVE('',#2307,#2308,#1938,.F.);
#2777=EDGE_CURVE('',#2285,#2307,#1939,.F.);
#2778=EDGE_CURVE('',#2308,#2285,#1940,.F.);
#2779=EDGE_CURVE('',#2309,#2300,#1941,.F.);
#2780=EDGE_CURVE('',#2299,#2309,#1942,.F.);
#2781=EDGE_CURVE('',#2310,#2309,#1467,.T.);
#2782=EDGE_CURVE('',#2300,#2311,#1468,.T.);
#2783=EDGE_CURVE('',#2311,#2310,#277,.T.);
#2784=EDGE_CURVE('',#2286,#2312,#1943,.F.);
#2785=EDGE_CURVE('',#2313,#2286,#1944,.F.);
#2786=EDGE_CURVE('',#2312,#2313,#1945,.F.);
#2787=EDGE_CURVE('',#2307,#2313,#1469,.T.);
#2788=EDGE_CURVE('',#2301,#2312,#1470,.T.);
#2789=EDGE_CURVE('',#2313,#2306,#1471,.T.);
#2790=EDGE_CURVE('',#2314,#2298,#1946,.F.);
#2791=EDGE_CURVE('',#2283,#2314,#1947,.F.);
#2792=EDGE_CURVE('',#2314,#2315,#1472,.T.);
#2793=EDGE_CURVE('',#2315,#2284,#278,.T.);
#2794=EDGE_CURVE('',#2312,#2294,#1473,.T.);
#2795=EDGE_CURVE('',#2309,#2314,#1474,.T.);
#2796=EDGE_CURVE('',#2315,#2308,#1475,.T.);
#2797=EDGE_CURVE('',#2308,#2304,#1476,.T.);
#2798=EDGE_CURVE('',#2305,#2307,#1477,.T.);
#2799=EDGE_CURVE('',#2311,#2303,#1478,.T.);
#2800=EDGE_CURVE('',#2304,#2310,#1479,.T.);
#2801=EDGE_CURVE('',#2315,#2310,#1480,.T.);
#2802=EDGE_CURVE('',#2289,#2297,#1948,.T.);
#2803=EDGE_CURVE('',#2316,#2316,#1949,.T.);
#2804=EDGE_CURVE('',#2317,#2317,#1950,.T.);
#2805=EDGE_CURVE('',#2317,#2316,#1481,.T.);
#2806=EDGE_CURVE('',#2318,#2318,#1951,.T.);
#2807=EDGE_CURVE('',#2318,#2319,#1482,.T.);
#2808=EDGE_CURVE('',#2319,#2319,#1952,.T.);
#2809=EDGE_CURVE('',#2320,#2320,#1953,.T.);
#2810=EDGE_CURVE('',#2321,#2321,#1954,.T.);
#2811=EDGE_CURVE('',#2321,#2322,#1483,.T.);
#2812=EDGE_CURVE('',#2322,#2322,#1955,.T.);
#2813=EDGE_CURVE('',#2323,#2323,#1956,.T.);
#2814=EDGE_CURVE('',#2323,#2324,#1484,.T.);
#2815=EDGE_CURVE('',#2324,#2324,#1957,.T.);
#2816=EDGE_CURVE('',#2325,#2325,#1958,.T.);
#2817=EDGE_CURVE('',#2325,#2326,#1485,.T.);
#2818=EDGE_CURVE('',#2326,#2326,#1959,.T.);
#2819=EDGE_CURVE('',#2327,#2327,#1960,.T.);
#2820=EDGE_CURVE('',#2328,#2328,#1961,.T.);
#2821=EDGE_CURVE('',#2328,#2329,#1486,.T.);
#2822=EDGE_CURVE('',#2329,#2329,#1962,.T.);
#2823=EDGE_CURVE('',#2330,#2330,#1963,.T.);
#2824=EDGE_CURVE('',#2330,#2320,#1487,.T.);
#2825=EDGE_CURVE('',#2327,#2331,#1488,.T.);
#2826=EDGE_CURVE('',#2331,#2331,#1964,.T.);
#2827=EDGE_CURVE('',#2332,#2333,#1965,.F.);
#2828=EDGE_CURVE('',#2334,#2332,#1966,.F.);
#2829=EDGE_CURVE('',#2333,#2334,#1967,.F.);
#2830=EDGE_CURVE('',#2335,#2336,#1968,.F.);
#2831=EDGE_CURVE('',#2337,#2335,#1969,.F.);
#2832=EDGE_CURVE('',#2336,#2337,#1970,.F.);
#2833=EDGE_CURVE('',#2338,#2339,#1971,.F.);
#2834=EDGE_CURVE('',#2340,#2338,#1972,.F.);
#2835=EDGE_CURVE('',#2339,#2340,#1973,.F.);
#2836=EDGE_CURVE('',#2341,#2342,#1974,.F.);
#2837=EDGE_CURVE('',#2343,#2341,#1975,.F.);
#2838=EDGE_CURVE('',#2342,#2343,#1976,.F.);
#2839=EDGE_CURVE('',#2341,#2334,#1489,.T.);
#2840=EDGE_CURVE('',#2332,#2343,#1490,.T.);
#2841=EDGE_CURVE('',#2344,#2345,#1977,.F.);
#2842=EDGE_CURVE('',#2346,#2344,#1978,.F.);
#2843=EDGE_CURVE('',#2345,#2346,#1979,.F.);
#2844=EDGE_CURVE('',#2347,#2348,#1980,.F.);
#2845=EDGE_CURVE('',#2349,#2347,#1981,.F.);
#2846=EDGE_CURVE('',#2348,#2349,#1982,.F.);
#2847=EDGE_CURVE('',#2347,#2337,#1491,.T.);
#2848=EDGE_CURVE('',#2335,#2349,#1492,.T.);
#2849=EDGE_CURVE('',#2350,#2351,#1983,.F.);
#2850=EDGE_CURVE('',#2352,#2350,#1984,.F.);
#2851=EDGE_CURVE('',#2351,#2352,#1985,.F.);
#2852=EDGE_CURVE('',#2350,#2340,#1493,.T.);
#2853=EDGE_CURVE('',#2338,#2352,#1494,.T.);
#2854=EDGE_CURVE('',#2342,#2351,#1495,.T.);
#2855=EDGE_CURVE('',#2352,#2341,#1496,.T.);
#2856=EDGE_CURVE('',#2353,#2354,#1986,.F.);
#2857=EDGE_CURVE('',#2355,#2353,#1987,.F.);
#2858=EDGE_CURVE('',#2354,#2355,#1988,.F.);
#2859=EDGE_CURVE('',#2344,#2355,#1497,.T.);
#2860=EDGE_CURVE('',#2353,#2346,#1498,.T.);
#2861=EDGE_CURVE('',#2351,#2354,#1499,.T.);
#2862=EDGE_CURVE('',#2355,#2350,#1500,.T.);
#2863=EDGE_CURVE('',#2354,#2348,#1501,.T.);
#2864=EDGE_CURVE('',#2349,#2353,#1502,.T.);
#2865=EDGE_CURVE('',#2348,#2342,#1503,.T.);
#2866=EDGE_CURVE('',#2343,#2347,#1504,.T.);
#2867=EDGE_CURVE('',#2336,#2345,#1505,.T.);
#2868=EDGE_CURVE('',#2346,#2335,#1506,.T.);
#2869=EDGE_CURVE('',#2345,#2339,#1507,.T.);
#2870=EDGE_CURVE('',#2340,#2344,#1508,.T.);
#2871=EDGE_CURVE('',#2339,#2333,#1509,.T.);
#2872=EDGE_CURVE('',#2334,#2338,#1510,.T.);
#2873=EDGE_CURVE('',#2333,#2336,#1511,.T.);
#2874=EDGE_CURVE('',#2337,#2332,#1512,.T.);
#2875=EDGE_CURVE('',#2356,#2356,#1989,.T.);
#2876=EDGE_CURVE('',#2357,#2357,#1990,.T.);
#2877=EDGE_CURVE('',#2357,#2358,#1513,.T.);
#2878=EDGE_CURVE('',#2358,#2358,#1991,.T.);
#2879=EDGE_CURVE('',#2356,#2359,#1514,.T.);
#2880=EDGE_CURVE('',#2359,#2359,#1992,.T.);
#2881=EDGE_CURVE('',#2360,#2360,#1993,.T.);
#2882=EDGE_CURVE('',#2360,#2361,#1994,.T.);
#2883=EDGE_CURVE('',#2361,#2361,#1995,.T.);
#2884=EDGE_CURVE('',#2362,#2362,#1996,.T.);
#2885=EDGE_CURVE('',#2362,#2363,#1515,.T.);
#2886=EDGE_CURVE('',#2363,#2363,#1997,.T.);
#2887=EDGE_CURVE('',#2362,#2364,#1516,.T.);
#2888=EDGE_CURVE('',#2364,#2365,#1998,.T.);
#2889=EDGE_CURVE('',#2365,#2364,#1999,.T.);
#2890=EDGE_CURVE('',#2365,#2366,#1517,.T.);
#2891=EDGE_CURVE('',#2366,#2366,#2000,.T.);
#2892=EDGE_CURVE('',#2367,#2367,#2001,.T.);
#2893=EDGE_CURVE('',#2367,#2361,#1518,.T.);
#2894=EDGE_CURVE('',#2360,#2368,#1519,.T.);
#2895=EDGE_CURVE('',#2368,#2368,#2002,.T.);
#2896=EDGE_CURVE('',#2369,#2370,#2003,.T.);
#2897=EDGE_CURVE('',#2371,#2371,#2004,.T.);
#2898=EDGE_CURVE('',#2371,#2372,#1520,.T.);
#2899=EDGE_CURVE('',#2372,#2372,#2005,.T.);
#2900=EDGE_CURVE('',#2373,#2373,#2006,.T.);
#2901=EDGE_CURVE('',#2373,#2374,#1521,.T.);
#2902=EDGE_CURVE('',#2374,#2374,#2007,.T.);
#2903=EDGE_CURVE('',#2373,#2375,#2008,.T.);
#2904=EDGE_CURVE('',#2375,#2375,#2009,.T.);
#2905=EDGE_CURVE('',#2376,#2376,#2010,.T.);
#2906=EDGE_CURVE('',#2376,#2375,#1522,.T.);
#2907=EDGE_CURVE('',#2377,#2378,#2011,.T.);
#2908=EDGE_CURVE('',#2378,#2377,#2012,.T.);
#2909=EDGE_CURVE('',#2378,#2379,#1523,.T.);
#2910=EDGE_CURVE('',#2379,#2379,#2013,.T.);
#2911=EDGE_CURVE('',#2371,#2377,#1524,.T.);
#2912=EDGE_CURVE('',#2380,#2381,#2014,.T.);
#2913=EDGE_CURVE('',#2382,#2383,#2015,.T.);
#2914=EDGE_CURVE('',#2384,#2385,#2016,.T.);
#2915=EDGE_CURVE('',#2386,#2387,#2017,.T.);
#2916=EDGE_CURVE('',#2388,#2389,#2018,.T.);
#2917=EDGE_CURVE('',#2390,#2391,#2019,.T.);
#2918=EDGE_CURVE('',#2392,#2393,#2020,.T.);
#2919=EDGE_CURVE('',#2394,#2395,#2021,.T.);
#2920=EDGE_CURVE('',#2396,#2397,#2022,.T.);
#2921=EDGE_CURVE('',#2398,#2398,#2023,.T.);
#2922=EDGE_CURVE('',#2398,#2399,#2024,.T.);
#2923=EDGE_CURVE('',#2399,#2399,#2025,.T.);
#2924=EDGE_CURVE('',#2400,#2401,#2026,.T.);
#2925=EDGE_CURVE('',#2402,#2402,#2027,.T.);
#2926=EDGE_CURVE('',#2403,#2403,#2028,.T.);
#2927=EDGE_CURVE('',#2404,#2404,#2029,.T.);
#2928=EDGE_CURVE('',#2404,#2405,#2030,.T.);
#2929=EDGE_CURVE('',#2405,#2405,#2031,.T.);
#2930=EDGE_CURVE('',#2406,#2407,#2032,.T.);
#2931=EDGE_CURVE('',#2408,#2408,#2033,.T.);
#2932=EDGE_CURVE('',#2409,#2409,#2034,.T.);
#2933=EDGE_CURVE('',#2410,#2410,#2035,.T.);
#2934=EDGE_CURVE('',#2410,#2411,#2036,.T.);
#2935=EDGE_CURVE('',#2411,#2411,#2037,.T.);
#2936=EDGE_CURVE('',#2412,#2413,#2038,.T.);
#2937=EDGE_CURVE('',#2414,#2414,#2039,.T.);
#2938=EDGE_CURVE('',#2415,#2415,#2040,.T.);
#2939=EDGE_CURVE('',#2416,#2416,#2041,.T.);
#2940=EDGE_CURVE('',#2416,#2417,#2042,.T.);
#2941=EDGE_CURVE('',#2417,#2417,#2043,.T.);
#2942=EDGE_CURVE('',#2418,#2419,#2044,.T.);
#2943=EDGE_CURVE('',#2420,#2420,#2045,.T.);
#2944=EDGE_CURVE('',#2421,#2421,#2046,.T.);
#2945=EDGE_CURVE('',#2422,#2422,#2047,.T.);
#2946=EDGE_CURVE('',#2422,#2423,#2048,.T.);
#2947=EDGE_CURVE('',#2423,#2423,#2049,.T.);
#2948=EDGE_CURVE('',#2424,#2425,#2050,.T.);
#2949=EDGE_CURVE('',#2426,#2426,#2051,.T.);
#2950=EDGE_CURVE('',#2427,#2427,#2052,.T.);
#2951=EDGE_CURVE('',#2428,#2428,#2053,.T.);
#2952=EDGE_CURVE('',#2428,#2429,#2054,.T.);
#2953=EDGE_CURVE('',#2429,#2429,#2055,.T.);
#2954=EDGE_CURVE('',#2430,#2431,#2056,.T.);
#2955=EDGE_CURVE('',#2432,#2432,#2057,.T.);
#2956=EDGE_CURVE('',#2433,#2433,#2058,.T.);
#2957=EDGE_CURVE('',#2434,#2434,#2059,.T.);
#2958=EDGE_CURVE('',#2434,#2435,#2060,.T.);
#2959=EDGE_CURVE('',#2435,#2435,#2061,.T.);
#2960=EDGE_CURVE('',#2436,#2437,#2062,.T.);
#2961=EDGE_CURVE('',#2438,#2438,#2063,.T.);
#2962=EDGE_CURVE('',#2439,#2439,#2064,.T.);
#2963=EDGE_CURVE('',#2440,#2440,#2065,.T.);
#2964=EDGE_CURVE('',#2440,#2441,#2066,.T.);
#2965=EDGE_CURVE('',#2441,#2441,#2067,.T.);
#2966=EDGE_CURVE('',#2442,#2443,#2068,.T.);
#2967=EDGE_CURVE('',#2444,#2444,#2069,.T.);
#2968=EDGE_CURVE('',#2445,#2445,#2070,.T.);
#2969=EDGE_CURVE('',#2446,#2446,#2071,.T.);
#2970=EDGE_CURVE('',#2446,#2447,#2072,.T.);
#2971=EDGE_CURVE('',#2447,#2447,#2073,.T.);
#2972=EDGE_CURVE('',#2448,#2449,#2074,.T.);
#2973=EDGE_CURVE('',#2450,#2450,#2075,.T.);
#2974=EDGE_CURVE('',#2451,#2451,#2076,.T.);
#2975=EDGE_CURVE('',#2452,#2452,#2077,.T.);
#2976=EDGE_CURVE('',#2452,#2453,#2078,.T.);
#2977=EDGE_CURVE('',#2453,#2453,#2079,.T.);
#2978=EDGE_CURVE('',#2454,#2455,#2080,.T.);
#2979=EDGE_CURVE('',#2456,#2456,#2081,.T.);
#2980=EDGE_CURVE('',#2457,#2457,#2082,.T.);
#2981=EDGE_CURVE('',#2458,#2458,#2083,.T.);
#2982=EDGE_CURVE('',#2458,#2459,#1525,.T.);
#2983=EDGE_CURVE('',#2459,#2459,#2084,.T.);
#2984=EDGE_CURVE('',#2460,#2460,#2085,.T.);
#2985=EDGE_CURVE('',#2460,#2461,#1526,.T.);
#2986=EDGE_CURVE('',#2461,#2461,#2086,.T.);
#2987=EDGE_CURVE('',#2462,#2462,#2087,.T.);
#2988=EDGE_CURVE('',#2462,#2463,#2088,.T.);
#2989=EDGE_CURVE('',#2463,#2463,#2089,.T.);
#2990=EDGE_CURVE('',#2464,#2465,#2090,.T.);
#2991=EDGE_CURVE('',#2466,#2466,#2091,.T.);
#2992=EDGE_CURVE('',#2467,#2467,#2092,.T.);
#2993=EDGE_CURVE('',#2468,#2468,#2093,.T.);
#2994=EDGE_CURVE('',#2468,#2469,#2094,.T.);
#2995=EDGE_CURVE('',#2469,#2469,#2095,.T.);
#2996=EDGE_CURVE('',#2470,#2471,#2096,.T.);
#2997=EDGE_CURVE('',#2472,#2472,#2097,.T.);
#2998=EDGE_CURVE('',#2473,#2473,#2098,.T.);
#2999=EDGE_CURVE('',#2474,#2475,#2099,.T.);
#3000=EDGE_CURVE('',#2476,#2477,#2100,.T.);
#3001=EDGE_CURVE('',#2478,#2478,#2101,.T.);
#3002=EDGE_CURVE('',#2478,#2479,#2102,.T.);
#3003=EDGE_CURVE('',#2479,#2480,#2103,.T.);
#3004=EDGE_CURVE('',#2480,#2479,#2104,.T.);
#3005=EDGE_CURVE('',#2481,#2482,#2105,.T.);
#3006=EDGE_CURVE('',#2482,#2483,#2106,.T.);
#3007=EDGE_CURVE('',#2483,#2483,#2107,.T.);
#3008=EDGE_CURVE('',#2482,#2481,#2108,.T.);
#3009=EDGE_CURVE('',#2484,#2485,#2109,.T.);
#3010=EDGE_CURVE('',#2485,#2484,#2110,.T.);
#3011=EDGE_CURVE('',#2485,#2481,#1527,.T.);
#3012=EDGE_CURVE('',#2486,#2486,#2111,.T.);
#3013=EDGE_CURVE('',#2486,#2484,#1528,.T.);
#3014=EDGE_CURVE('',#2487,#2487,#2112,.T.);
#3015=EDGE_CURVE('',#2487,#2488,#1529,.T.);
#3016=EDGE_CURVE('',#2488,#2488,#2113,.T.);
#3017=EDGE_CURVE('',#2480,#2488,#1530,.T.);
#3018=EDGE_CURVE('',#2489,#2489,#2114,.T.);
#3019=EDGE_CURVE('',#2489,#2490,#2115,.T.);
#3020=EDGE_CURVE('',#2490,#2490,#2116,.T.);
#3021=EDGE_CURVE('',#2491,#2491,#2117,.T.);
#3022=EDGE_CURVE('',#2491,#2492,#2118,.T.);
#3023=EDGE_CURVE('',#2492,#2492,#2119,.T.);
#3024=EDGE_CURVE('',#2493,#2494,#2120,.T.);
#3025=EDGE_CURVE('',#2494,#2493,#2121,.T.);
#3026=EDGE_CURVE('',#2494,#2492,#1531,.T.);
#3027=EDGE_CURVE('',#2495,#2495,#2122,.T.);
#3028=EDGE_CURVE('',#2495,#2493,#1532,.T.);
#3029=EDGE_CURVE('',#2496,#2496,#2123,.T.);
#3030=EDGE_CURVE('',#2496,#2497,#1533,.T.);
#3031=EDGE_CURVE('',#2497,#2497,#2124,.T.);
#3032=EDGE_CURVE('',#2489,#2497,#1534,.T.);
#3033=EDGE_CURVE('',#2498,#2498,#2125,.T.);
#3034=EDGE_CURVE('',#2498,#2499,#1535,.T.);
#3035=EDGE_CURVE('',#2499,#2499,#2126,.T.);
#3036=EDGE_CURVE('',#2500,#2500,#2127,.T.);
#3037=EDGE_CURVE('',#2500,#2501,#2128,.T.);
#3038=EDGE_CURVE('',#2501,#2501,#2129,.T.);
#3039=EDGE_CURVE('',#2502,#2503,#1536,.T.);
#3040=EDGE_CURVE('',#2503,#2504,#1537,.T.);
#3041=EDGE_CURVE('',#2504,#2505,#1538,.T.);
#3042=EDGE_CURVE('',#2505,#2506,#1539,.T.);
#3043=EDGE_CURVE('',#2506,#2507,#1540,.T.);
#3044=EDGE_CURVE('',#2507,#2502,#1541,.T.);
#3045=EDGE_CURVE('',#2508,#2508,#2130,.T.);
#3046=EDGE_CURVE('',#2508,#2500,#1542,.T.);
#3047=EDGE_CURVE('',#2509,#2510,#1543,.T.);
#3048=EDGE_CURVE('',#2511,#2509,#1544,.T.);
#3049=EDGE_CURVE('',#2511,#2510,#1545,.T.);
#3050=EDGE_CURVE('',#2512,#2511,#1546,.T.);
#3051=EDGE_CURVE('',#2512,#2510,#1547,.T.);
#3052=EDGE_CURVE('',#2513,#2512,#1548,.T.);
#3053=EDGE_CURVE('',#2513,#2510,#1549,.T.);
#3054=EDGE_CURVE('',#2514,#2513,#1550,.T.);
#3055=EDGE_CURVE('',#2514,#2510,#1551,.T.);
#3056=EDGE_CURVE('',#2515,#2514,#1552,.T.);
#3057=EDGE_CURVE('',#2515,#2510,#1553,.T.);
#3058=EDGE_CURVE('',#2509,#2515,#1554,.T.);
#3059=EDGE_CURVE('',#2502,#2511,#1555,.T.);
#3060=EDGE_CURVE('',#2503,#2509,#1556,.T.);
#3061=EDGE_CURVE('',#2507,#2512,#1557,.T.);
#3062=EDGE_CURVE('',#2506,#2513,#1558,.T.);
#3063=EDGE_CURVE('',#2505,#2514,#1559,.T.);
#3064=EDGE_CURVE('',#2504,#2515,#1560,.T.);
#3065=EDGE_CURVE('',#2498,#2516,#1561,.T.);
#3066=EDGE_CURVE('',#2516,#2516,#2131,.F.);
#3067=EDGE_CURVE('',#2517,#2517,#2132,.T.);
#3068=EDGE_CURVE('',#2517,#2518,#1562,.T.);
#3069=EDGE_CURVE('',#2518,#2518,#2133,.T.);
#3070=EDGE_CURVE('',#2519,#2519,#2134,.T.);
#3071=EDGE_CURVE('',#2519,#2520,#1563,.T.);
#3072=EDGE_CURVE('',#2520,#2520,#2135,.T.);
#3073=EDGE_CURVE('',#2521,#2521,#2136,.T.);
#3074=EDGE_CURVE('',#2521,#2522,#1564,.T.);
#3075=EDGE_CURVE('',#2522,#2522,#2137,.T.);
#3076=EDGE_CURVE('',#2523,#2523,#2138,.T.);
#3077=EDGE_CURVE('',#2524,#2524,#2139,.T.);
#3078=EDGE_CURVE('',#2524,#2523,#1565,.T.);
#3079=EDGE_CURVE('',#2525,#2525,#2140,.T.);
#3080=EDGE_CURVE('',#2525,#2526,#1566,.T.);
#3081=EDGE_CURVE('',#2526,#2526,#2141,.T.);
#3082=EDGE_CURVE('',#2527,#2527,#2142,.T.);
#3083=EDGE_CURVE('',#2527,#2528,#1567,.T.);
#3084=EDGE_CURVE('',#2528,#2528,#2143,.T.);
#3085=EDGE_CURVE('',#2529,#2529,#2144,.T.);
#3086=EDGE_CURVE('',#2530,#2530,#2145,.T.);
#3087=EDGE_CURVE('',#2530,#2529,#1568,.T.);
#3088=EDGE_CURVE('',#2531,#2531,#2146,.T.);
#3089=EDGE_CURVE('',#2531,#2532,#2147,.T.);
#3090=EDGE_CURVE('',#2532,#2532,#2148,.T.);
#3091=EDGE_CURVE('',#2533,#2533,#2149,.T.);
#3092=EDGE_CURVE('',#2533,#2534,#1569,.T.);
#3093=EDGE_CURVE('',#2534,#2534,#2150,.T.);
#3094=EDGE_CURVE('',#2535,#2536,#2151,.T.);
#3095=EDGE_CURVE('',#2536,#2535,#2152,.T.);
#3096=EDGE_CURVE('',#2536,#2533,#1570,.T.);
#3097=EDGE_CURVE('',#2535,#2537,#1571,.T.);
#3098=EDGE_CURVE('',#2537,#2537,#2153,.T.);
#3099=EDGE_CURVE('',#2532,#2538,#1572,.T.);
#3100=EDGE_CURVE('',#2538,#2538,#2154,.T.);
#3101=EDGE_CURVE('',#2539,#2539,#2155,.T.);
#3102=EDGE_CURVE('',#2539,#2531,#1573,.T.);
#3103=EDGE_CURVE('',#2540,#2541,#2156,.T.);
#3104=EDGE_CURVE('',#2542,#2542,#2157,.T.);
#3105=EDGE_CURVE('',#2542,#2543,#1574,.T.);
#3106=EDGE_CURVE('',#2543,#2543,#2158,.T.);
#3107=EDGE_CURVE('',#2544,#2544,#2159,.T.);
#3108=EDGE_CURVE('',#2544,#2545,#1575,.T.);
#3109=EDGE_CURVE('',#2545,#2545,#2160,.T.);
#3110=EDGE_CURVE('',#2545,#2546,#2161,.T.);
#3111=EDGE_CURVE('',#2546,#2546,#2162,.T.);
#3112=EDGE_CURVE('',#2546,#2547,#1576,.T.);
#3113=EDGE_CURVE('',#2547,#2547,#2163,.T.);
#3114=EDGE_CURVE('',#2548,#2549,#2164,.T.);
#3115=EDGE_CURVE('',#2549,#2550,#1577,.T.);
#3116=EDGE_CURVE('',#2550,#2550,#2165,.T.);
#3117=EDGE_CURVE('',#2549,#2548,#2166,.T.);
#3118=EDGE_CURVE('',#2548,#2542,#1578,.T.);
#3119=EDGE_CURVE('',#2551,#2552,#2167,.T.);
#3120=EDGE_CURVE('',#2553,#2554,#2168,.T.);
#3121=EDGE_CURVE('',#2555,#2556,#2169,.T.);
#3122=EDGE_CURVE('',#2557,#2558,#2170,.T.);
#3123=EDGE_CURVE('',#2559,#2560,#2171,.T.);
#3124=EDGE_CURVE('',#2561,#2562,#2172,.T.);
#3125=EDGE_CURVE('',#2563,#2564,#2173,.T.);
#3126=EDGE_CURVE('',#2565,#2565,#2174,.T.);
#3127=EDGE_CURVE('',#2565,#2566,#2175,.T.);
#3128=EDGE_CURVE('',#2566,#2566,#2176,.T.);
#3129=EDGE_CURVE('',#2567,#2568,#2177,.T.);
#3130=EDGE_CURVE('',#2569,#2569,#2178,.T.);
#3131=EDGE_CURVE('',#2570,#2570,#2179,.T.);
#3132=EDGE_CURVE('',#2571,#2571,#2180,.T.);
#3133=EDGE_CURVE('',#2571,#2572,#2181,.T.);
#3134=EDGE_CURVE('',#2572,#2572,#2182,.T.);
#3135=EDGE_CURVE('',#2573,#2574,#2183,.T.);
#3136=EDGE_CURVE('',#2575,#2575,#2184,.T.);
#3137=EDGE_CURVE('',#2576,#2576,#2185,.T.);
#3138=EDGE_CURVE('',#2577,#2577,#2186,.T.);
#3139=EDGE_CURVE('',#2577,#2578,#2187,.T.);
#3140=EDGE_CURVE('',#2578,#2578,#2188,.T.);
#3141=EDGE_CURVE('',#2579,#2580,#2189,.T.);
#3142=EDGE_CURVE('',#2581,#2581,#2190,.T.);
#3143=EDGE_CURVE('',#2582,#2582,#2191,.T.);
#3144=EDGE_CURVE('',#2583,#2583,#2192,.T.);
#3145=EDGE_CURVE('',#2583,#2584,#2193,.T.);
#3146=EDGE_CURVE('',#2584,#2584,#2194,.T.);
#3147=EDGE_CURVE('',#2585,#2586,#2195,.T.);
#3148=EDGE_CURVE('',#2587,#2587,#2196,.T.);
#3149=EDGE_CURVE('',#2588,#2588,#2197,.T.);
#3150=EDGE_CURVE('',#2589,#2589,#2198,.T.);
#3151=EDGE_CURVE('',#2589,#2590,#2199,.T.);
#3152=EDGE_CURVE('',#2590,#2590,#2200,.T.);
#3153=EDGE_CURVE('',#2591,#2592,#2201,.T.);
#3154=EDGE_CURVE('',#2593,#2593,#2202,.T.);
#3155=EDGE_CURVE('',#2594,#2594,#2203,.T.);
#3156=EDGE_CURVE('',#2595,#2595,#2204,.T.);
#3157=EDGE_CURVE('',#2595,#2596,#2205,.T.);
#3158=EDGE_CURVE('',#2596,#2596,#2206,.T.);
#3159=EDGE_CURVE('',#2597,#2598,#2207,.T.);
#3160=EDGE_CURVE('',#2599,#2599,#2208,.T.);
#3161=EDGE_CURVE('',#2600,#2600,#2209,.T.);
#3162=EDGE_CURVE('',#2601,#2601,#2210,.T.);
#3163=EDGE_CURVE('',#2601,#2602,#2211,.T.);
#3164=EDGE_CURVE('',#2602,#2602,#2212,.T.);
#3165=EDGE_CURVE('',#2603,#2604,#2213,.T.);
#3166=EDGE_CURVE('',#2605,#2605,#2214,.T.);
#3167=EDGE_CURVE('',#2606,#2606,#2215,.T.);
#3168=EDGE_CURVE('',#2607,#2607,#2216,.T.);
#3169=EDGE_CURVE('',#2607,#2608,#2217,.T.);
#3170=EDGE_CURVE('',#2608,#2608,#2218,.T.);
#3171=EDGE_CURVE('',#2609,#2610,#2219,.T.);
#3172=EDGE_CURVE('',#2611,#2611,#2220,.T.);
#3173=EDGE_CURVE('',#2612,#2612,#2221,.T.);
#3174=EDGE_CURVE('',#2613,#2613,#2222,.T.);
#3175=EDGE_CURVE('',#2613,#2614,#1579,.T.);
#3176=EDGE_CURVE('',#2614,#2614,#2223,.T.);
#3177=EDGE_CURVE('',#2615,#2615,#2224,.T.);
#3178=EDGE_CURVE('',#2615,#2616,#1580,.T.);
#3179=EDGE_CURVE('',#2616,#2616,#2225,.T.);
#3180=EDGE_CURVE('',#2617,#2617,#2226,.T.);
#3181=EDGE_CURVE('',#2617,#2618,#2227,.T.);
#3182=EDGE_CURVE('',#2619,#2618,#2228,.T.);
#3183=EDGE_CURVE('',#2618,#2619,#2229,.T.);
#3184=EDGE_CURVE('',#2620,#2621,#2230,.T.);
#3185=EDGE_CURVE('',#2621,#2620,#2231,.T.);
#3186=EDGE_CURVE('',#2621,#2622,#2232,.T.);
#3187=EDGE_CURVE('',#2622,#2622,#2233,.T.);
#3188=EDGE_CURVE('',#2620,#2623,#1581,.T.);
#3189=EDGE_CURVE('',#2623,#2624,#2234,.T.);
#3190=EDGE_CURVE('',#2624,#2623,#2235,.T.);
#3191=EDGE_CURVE('',#2625,#2625,#2236,.T.);
#3192=EDGE_CURVE('',#2625,#2624,#1582,.T.);
#3193=EDGE_CURVE('',#2626,#2626,#2237,.T.);
#3194=EDGE_CURVE('',#2626,#2627,#1583,.T.);
#3195=EDGE_CURVE('',#2627,#2627,#2238,.T.);
#3196=EDGE_CURVE('',#2627,#2619,#1584,.T.);
#3197=EDGE_CURVE('',#2628,#2628,#2239,.T.);
#3198=EDGE_CURVE('',#2628,#2629,#2240,.T.);
#3199=EDGE_CURVE('',#2629,#2629,#2241,.T.);
#3200=EDGE_CURVE('',#2630,#2630,#2242,.T.);
#3201=EDGE_CURVE('',#2630,#2631,#2243,.T.);
#3202=EDGE_CURVE('',#2631,#2631,#2244,.T.);
#3203=EDGE_CURVE('',#2631,#2632,#1585,.T.);
#3204=EDGE_CURVE('',#2632,#2633,#2245,.T.);
#3205=EDGE_CURVE('',#2633,#2632,#2246,.T.);
#3206=EDGE_CURVE('',#2634,#2634,#2247,.T.);
#3207=EDGE_CURVE('',#2634,#2633,#1586,.T.);
#3208=EDGE_CURVE('',#2635,#2635,#2248,.T.);
#3209=EDGE_CURVE('',#2635,#2636,#1587,.T.);
#3210=EDGE_CURVE('',#2636,#2636,#2249,.T.);
#3211=EDGE_CURVE('',#2636,#2628,#1588,.T.);
#3212=EDGE_CURVE('',#2637,#2637,#2250,.T.);
#3213=EDGE_CURVE('',#2637,#2638,#1589,.T.);
#3214=EDGE_CURVE('',#2639,#2638,#79,.T.);
#3215=EDGE_CURVE('',#2638,#2639,#80,.T.);
#3216=EDGE_CURVE('',#2640,#2641,#81,.T.);
#3217=EDGE_CURVE('',#2641,#2640,#82,.T.);
#3218=EDGE_CURVE('',#2641,#2642,#1590,.T.);
#3219=EDGE_CURVE('',#2642,#2642,#2251,.T.);
#3220=EDGE_CURVE('',#2643,#2643,#2252,.T.);
#3221=EDGE_CURVE('',#2643,#2644,#1591,.T.);
#3222=EDGE_CURVE('',#2645,#2644,#83,.T.);
#3223=EDGE_CURVE('',#2644,#2645,#84,.T.);
#3224=EDGE_CURVE('',#2646,#2647,#85,.T.);
#3225=EDGE_CURVE('',#2647,#2646,#86,.T.);
#3226=EDGE_CURVE('',#2647,#2648,#1592,.T.);
#3227=EDGE_CURVE('',#2648,#2648,#2253,.T.);
#3228=EDGE_CURVE('',#2649,#2649,#2254,.T.);
#3229=EDGE_CURVE('',#2649,#2650,#1593,.T.);
#3230=EDGE_CURVE('',#2651,#2650,#87,.T.);
#3231=EDGE_CURVE('',#2650,#2651,#88,.T.);
#3232=EDGE_CURVE('',#2652,#2653,#89,.T.);
#3233=EDGE_CURVE('',#2653,#2652,#90,.T.);
#3234=EDGE_CURVE('',#2653,#2654,#1594,.T.);
#3235=EDGE_CURVE('',#2654,#2654,#2255,.T.);
#3236=EDGE_CURVE('',#2655,#2655,#2256,.T.);
#3237=EDGE_CURVE('',#2655,#2656,#1595,.T.);
#3238=EDGE_CURVE('',#2657,#2656,#91,.T.);
#3239=EDGE_CURVE('',#2656,#2657,#92,.T.);
#3240=EDGE_CURVE('',#2658,#2659,#93,.T.);
#3241=EDGE_CURVE('',#2659,#2658,#94,.T.);
#3242=EDGE_CURVE('',#2659,#2660,#1596,.T.);
#3243=EDGE_CURVE('',#2660,#2660,#2257,.T.);
#3244=EDGE_CURVE('',#2661,#2662,#1597,.T.);
#3245=EDGE_CURVE('',#2661,#2663,#1598,.T.);
#3246=EDGE_CURVE('',#2664,#2663,#1599,.T.);
#3247=EDGE_CURVE('',#2662,#2664,#1600,.T.);
#3248=EDGE_CURVE('',#2665,#2661,#1601,.T.);
#3249=EDGE_CURVE('',#2665,#2666,#1602,.T.);
#3250=EDGE_CURVE('',#2663,#2666,#1603,.T.);
#3251=EDGE_CURVE('',#2667,#2665,#1604,.T.);
#3252=EDGE_CURVE('',#2668,#2667,#1605,.T.);
#3253=EDGE_CURVE('',#2666,#2668,#1606,.T.);
#3254=EDGE_CURVE('',#2664,#2669,#1607,.T.);
#3255=EDGE_CURVE('',#2670,#2669,#1608,.T.);
#3256=EDGE_CURVE('',#2670,#2662,#1609,.T.);
#3257=EDGE_CURVE('',#2667,#2671,#1610,.T.);
#3258=EDGE_CURVE('',#2671,#2672,#1611,.T.);
#3259=EDGE_CURVE('',#2672,#2668,#1612,.T.);
#3260=EDGE_CURVE('',#2673,#2670,#1613,.T.);
#3261=EDGE_CURVE('',#2673,#2674,#1614,.T.);
#3262=EDGE_CURVE('',#2675,#2674,#1615,.T.);
#3263=EDGE_CURVE('',#2676,#2675,#1616,.T.);
#3264=EDGE_CURVE('',#2676,#2677,#1617,.T.);
#3265=EDGE_CURVE('',#2677,#2678,#1618,.T.);
#3266=EDGE_CURVE('',#2678,#2679,#1619,.T.);
#3267=EDGE_CURVE('',#2680,#2679,#1620,.T.);
#3268=EDGE_CURVE('',#2680,#2681,#1621,.T.);
#3269=EDGE_CURVE('',#2681,#2682,#1622,.T.);
#3270=EDGE_CURVE('',#2682,#2683,#1623,.T.);
#3271=EDGE_CURVE('',#2684,#2683,#1624,.T.);
#3272=EDGE_CURVE('',#2685,#2684,#1625,.T.);
#3273=EDGE_CURVE('',#2686,#2685,#1626,.T.);
#3274=EDGE_CURVE('',#2687,#2686,#1627,.T.);
#3275=EDGE_CURVE('',#2688,#2687,#1628,.T.);
#3276=EDGE_CURVE('',#2688,#2689,#1629,.T.);
#3277=EDGE_CURVE('',#2689,#2690,#1630,.T.);
#3278=EDGE_CURVE('',#2690,#2671,#1631,.T.);
#3279=EDGE_CURVE('',#2691,#2691,#2258,.T.);
#3280=EDGE_CURVE('',#2692,#2692,#2259,.T.);
#3281=EDGE_CURVE('',#2693,#2693,#2260,.T.);
#3282=EDGE_CURVE('',#2694,#2688,#1632,.T.);
#3283=EDGE_CURVE('',#2695,#2694,#1633,.T.);
#3284=EDGE_CURVE('',#2689,#2695,#1634,.T.);
#3285=EDGE_CURVE('',#2696,#2695,#1635,.T.);
#3286=EDGE_CURVE('',#2690,#2696,#1636,.T.);
#3287=EDGE_CURVE('',#2672,#2696,#1637,.T.);
#3288=EDGE_CURVE('',#2697,#2694,#1638,.T.);
#3289=EDGE_CURVE('',#2698,#2697,#1639,.T.);
#3290=EDGE_CURVE('',#2699,#2698,#1640,.T.);
#3291=EDGE_CURVE('',#2700,#2699,#1641,.T.);
#3292=EDGE_CURVE('',#2701,#2700,#1642,.T.);
#3293=EDGE_CURVE('',#2701,#2702,#1643,.T.);
#3294=EDGE_CURVE('',#2702,#2703,#1644,.T.);
#3295=EDGE_CURVE('',#2703,#2704,#1645,.T.);
#3296=EDGE_CURVE('',#2705,#2704,#1646,.T.);
#3297=EDGE_CURVE('',#2705,#2706,#1647,.T.);
#3298=EDGE_CURVE('',#2706,#2707,#1648,.T.);
#3299=EDGE_CURVE('',#2707,#2708,#1649,.T.);
#3300=EDGE_CURVE('',#2709,#2708,#1650,.T.);
#3301=EDGE_CURVE('',#2710,#2709,#1651,.T.);
#3302=EDGE_CURVE('',#2711,#2710,#1652,.T.);
#3303=EDGE_CURVE('',#2669,#2711,#1653,.T.);
#3304=EDGE_CURVE('',#2712,#2712,#2261,.T.);
#3305=EDGE_CURVE('',#2713,#2713,#2262,.T.);
#3306=EDGE_CURVE('',#2714,#2714,#2263,.T.);
#3307=EDGE_CURVE('',#2697,#2687,#1654,.T.);
#3308=EDGE_CURVE('',#2708,#2676,#1655,.T.);
#3309=EDGE_CURVE('',#2677,#2707,#1656,.T.);
#3310=EDGE_CURVE('',#2678,#2706,#1657,.T.);
#3311=EDGE_CURVE('',#2679,#2705,#1658,.T.);
#3312=EDGE_CURVE('',#2709,#2675,#1659,.T.);
#3313=EDGE_CURVE('',#2704,#2680,#1660,.T.);
#3314=EDGE_CURVE('',#2682,#2702,#1661,.T.);
#3315=EDGE_CURVE('',#2683,#2701,#1662,.T.);
#3316=EDGE_CURVE('',#2681,#2703,#1663,.T.);
#3317=EDGE_CURVE('',#2684,#2700,#1664,.T.);
#3318=EDGE_CURVE('',#2691,#2712,#1665,.T.);
#3319=EDGE_CURVE('',#2713,#2692,#1666,.T.);
#3320=EDGE_CURVE('',#2714,#2693,#1667,.T.);
#3321=EDGE_CURVE('',#2686,#2698,#1668,.T.);
#3322=EDGE_CURVE('',#2699,#2685,#1669,.T.);
#3323=EDGE_CURVE('',#2711,#2673,#1670,.T.);
#3324=EDGE_CURVE('',#2674,#2710,#1671,.T.);
#3325=ORIENTED_EDGE('',*,*,#2715,.F.);
#3326=ORIENTED_EDGE('',*,*,#2716,.T.);
#3327=ORIENTED_EDGE('',*,*,#2717,.T.);
#3328=ORIENTED_EDGE('',*,*,#2716,.F.);
#3329=ORIENTED_EDGE('',*,*,#2717,.F.);
#3330=ORIENTED_EDGE('',*,*,#2718,.F.);
#3331=ORIENTED_EDGE('',*,*,#2719,.F.);
#3332=ORIENTED_EDGE('',*,*,#2720,.T.);
#3333=ORIENTED_EDGE('',*,*,#2721,.T.);
#3334=ORIENTED_EDGE('',*,*,#2720,.F.);
#3335=ORIENTED_EDGE('',*,*,#2721,.F.);
#3336=ORIENTED_EDGE('',*,*,#2722,.F.);
#3337=ORIENTED_EDGE('',*,*,#2723,.T.);
#3338=ORIENTED_EDGE('',*,*,#2724,.T.);
#3339=ORIENTED_EDGE('',*,*,#2723,.F.);
#3340=ORIENTED_EDGE('',*,*,#2724,.F.);
#3341=ORIENTED_EDGE('',*,*,#2725,.F.);
#3342=ORIENTED_EDGE('',*,*,#2726,.T.);
#3343=ORIENTED_EDGE('',*,*,#2727,.T.);
#3344=ORIENTED_EDGE('',*,*,#2726,.F.);
#3345=ORIENTED_EDGE('',*,*,#2727,.F.);
#3346=ORIENTED_EDGE('',*,*,#2728,.F.);
#3347=ORIENTED_EDGE('',*,*,#2728,.T.);
#3348=ORIENTED_EDGE('',*,*,#2729,.T.);
#3349=ORIENTED_EDGE('',*,*,#2730,.F.);
#3350=ORIENTED_EDGE('',*,*,#2729,.F.);
#3351=ORIENTED_EDGE('',*,*,#2731,.F.);
#3352=ORIENTED_EDGE('',*,*,#2732,.T.);
#3353=ORIENTED_EDGE('',*,*,#2733,.T.);
#3354=ORIENTED_EDGE('',*,*,#2732,.F.);
#3355=ORIENTED_EDGE('',*,*,#2733,.F.);
#3356=ORIENTED_EDGE('',*,*,#2718,.T.);
#3357=ORIENTED_EDGE('',*,*,#2734,.T.);
#3358=ORIENTED_EDGE('',*,*,#2735,.F.);
#3359=ORIENTED_EDGE('',*,*,#2734,.F.);
#3360=ORIENTED_EDGE('',*,*,#2736,.F.);
#3361=ORIENTED_EDGE('',*,*,#2737,.F.);
#3362=ORIENTED_EDGE('',*,*,#2738,.F.);
#3363=ORIENTED_EDGE('',*,*,#2739,.F.);
#3364=ORIENTED_EDGE('',*,*,#2739,.T.);
#3365=ORIENTED_EDGE('',*,*,#2740,.T.);
#3366=ORIENTED_EDGE('',*,*,#2741,.F.);
#3367=ORIENTED_EDGE('',*,*,#2742,.F.);
#3368=ORIENTED_EDGE('',*,*,#2743,.F.);
#3369=ORIENTED_EDGE('',*,*,#2744,.F.);
#3370=ORIENTED_EDGE('',*,*,#2745,.F.);
#3371=ORIENTED_EDGE('',*,*,#2746,.T.);
#3372=ORIENTED_EDGE('',*,*,#2735,.T.);
#3373=ORIENTED_EDGE('',*,*,#2738,.T.);
#3374=ORIENTED_EDGE('',*,*,#2747,.F.);
#3375=ORIENTED_EDGE('',*,*,#2748,.F.);
#3376=ORIENTED_EDGE('',*,*,#2749,.F.);
#3377=ORIENTED_EDGE('',*,*,#2750,.F.);
#3378=ORIENTED_EDGE('',*,*,#2751,.F.);
#3379=ORIENTED_EDGE('',*,*,#2752,.F.);
#3380=ORIENTED_EDGE('',*,*,#2740,.F.);
#3381=ORIENTED_EDGE('',*,*,#2731,.T.);
#3382=ORIENTED_EDGE('',*,*,#2737,.T.);
#3383=ORIENTED_EDGE('',*,*,#2753,.T.);
#3384=ORIENTED_EDGE('',*,*,#2754,.F.);
#3385=ORIENTED_EDGE('',*,*,#2747,.T.);
#3386=ORIENTED_EDGE('',*,*,#2736,.T.);
#3387=ORIENTED_EDGE('',*,*,#2746,.F.);
#3388=ORIENTED_EDGE('',*,*,#2755,.F.);
#3389=ORIENTED_EDGE('',*,*,#2756,.F.);
#3390=ORIENTED_EDGE('',*,*,#2757,.F.);
#3391=ORIENTED_EDGE('',*,*,#2758,.F.);
#3392=ORIENTED_EDGE('',*,*,#2759,.F.);
#3393=ORIENTED_EDGE('',*,*,#2753,.F.);
#3394=ORIENTED_EDGE('',*,*,#2730,.T.);
#3395=ORIENTED_EDGE('',*,*,#2752,.T.);
#3396=ORIENTED_EDGE('',*,*,#2760,.T.);
#3397=ORIENTED_EDGE('',*,*,#2761,.T.);
#3398=ORIENTED_EDGE('',*,*,#2741,.T.);
#3399=ORIENTED_EDGE('',*,*,#2751,.T.);
#3400=ORIENTED_EDGE('',*,*,#2762,.F.);
#3401=ORIENTED_EDGE('',*,*,#2763,.F.);
#3402=ORIENTED_EDGE('',*,*,#2760,.F.);
#3403=ORIENTED_EDGE('',*,*,#2719,.T.);
#3404=ORIENTED_EDGE('',*,*,#2722,.T.);
#3405=ORIENTED_EDGE('',*,*,#2750,.T.);
#3406=ORIENTED_EDGE('',*,*,#2764,.T.);
#3407=ORIENTED_EDGE('',*,*,#2765,.T.);
#3408=ORIENTED_EDGE('',*,*,#2762,.T.);
#3409=ORIENTED_EDGE('',*,*,#2757,.T.);
#3410=ORIENTED_EDGE('',*,*,#2766,.T.);
#3411=ORIENTED_EDGE('',*,*,#2767,.T.);
#3412=ORIENTED_EDGE('',*,*,#2768,.T.);
#3413=ORIENTED_EDGE('',*,*,#2769,.F.);
#3414=ORIENTED_EDGE('',*,*,#2770,.F.);
#3415=ORIENTED_EDGE('',*,*,#2771,.F.);
#3416=ORIENTED_EDGE('',*,*,#2772,.F.);
#3417=ORIENTED_EDGE('',*,*,#2773,.F.);
#3418=ORIENTED_EDGE('',*,*,#2767,.F.);
#3419=ORIENTED_EDGE('',*,*,#2773,.T.);
#3420=ORIENTED_EDGE('',*,*,#2774,.T.);
#3421=ORIENTED_EDGE('',*,*,#2770,.T.);
#3422=ORIENTED_EDGE('',*,*,#2775,.T.);
#3423=ORIENTED_EDGE('',*,*,#2776,.F.);
#3424=ORIENTED_EDGE('',*,*,#2777,.F.);
#3425=ORIENTED_EDGE('',*,*,#2778,.F.);
#3426=ORIENTED_EDGE('',*,*,#2765,.F.);
#3427=ORIENTED_EDGE('',*,*,#2779,.F.);
#3428=ORIENTED_EDGE('',*,*,#2780,.F.);
#3429=ORIENTED_EDGE('',*,*,#2781,.T.);
#3430=ORIENTED_EDGE('',*,*,#2779,.T.);
#3431=ORIENTED_EDGE('',*,*,#2782,.T.);
#3432=ORIENTED_EDGE('',*,*,#2783,.T.);
#3433=ORIENTED_EDGE('',*,*,#2784,.F.);
#3434=ORIENTED_EDGE('',*,*,#2785,.F.);
#3435=ORIENTED_EDGE('',*,*,#2786,.F.);
#3436=ORIENTED_EDGE('',*,*,#2777,.T.);
#3437=ORIENTED_EDGE('',*,*,#2787,.T.);
#3438=ORIENTED_EDGE('',*,*,#2785,.T.);
#3439=ORIENTED_EDGE('',*,*,#2744,.T.);
#3440=ORIENTED_EDGE('',*,*,#2772,.T.);
#3441=ORIENTED_EDGE('',*,*,#2788,.T.);
#3442=ORIENTED_EDGE('',*,*,#2786,.T.);
#3443=ORIENTED_EDGE('',*,*,#2789,.T.);
#3444=ORIENTED_EDGE('',*,*,#2790,.F.);
#3445=ORIENTED_EDGE('',*,*,#2791,.F.);
#3446=ORIENTED_EDGE('',*,*,#2761,.F.);
#3447=ORIENTED_EDGE('',*,*,#2742,.T.);
#3448=ORIENTED_EDGE('',*,*,#2791,.T.);
#3449=ORIENTED_EDGE('',*,*,#2792,.T.);
#3450=ORIENTED_EDGE('',*,*,#2793,.T.);
#3451=ORIENTED_EDGE('',*,*,#2755,.T.);
#3452=ORIENTED_EDGE('',*,*,#2745,.T.);
#3453=ORIENTED_EDGE('',*,*,#2784,.T.);
#3454=ORIENTED_EDGE('',*,*,#2794,.T.);
#3455=ORIENTED_EDGE('',*,*,#2790,.T.);
#3456=ORIENTED_EDGE('',*,*,#2763,.T.);
#3457=ORIENTED_EDGE('',*,*,#2780,.T.);
#3458=ORIENTED_EDGE('',*,*,#2795,.T.);
#3459=ORIENTED_EDGE('',*,*,#2796,.T.);
#3460=ORIENTED_EDGE('',*,*,#2778,.T.);
#3461=ORIENTED_EDGE('',*,*,#2743,.T.);
#3462=ORIENTED_EDGE('',*,*,#2793,.F.);
#3463=ORIENTED_EDGE('',*,*,#2776,.T.);
#3464=ORIENTED_EDGE('',*,*,#2797,.T.);
#3465=ORIENTED_EDGE('',*,*,#2771,.T.);
#3466=ORIENTED_EDGE('',*,*,#2798,.T.);
#3467=ORIENTED_EDGE('',*,*,#2799,.T.);
#3468=ORIENTED_EDGE('',*,*,#2769,.T.);
#3469=ORIENTED_EDGE('',*,*,#2800,.T.);
#3470=ORIENTED_EDGE('',*,*,#2783,.F.);
#3471=ORIENTED_EDGE('',*,*,#2800,.F.);
#3472=ORIENTED_EDGE('',*,*,#2797,.F.);
#3473=ORIENTED_EDGE('',*,*,#2796,.F.);
#3474=ORIENTED_EDGE('',*,*,#2801,.T.);
#3475=ORIENTED_EDGE('',*,*,#2758,.T.);
#3476=ORIENTED_EDGE('',*,*,#2768,.F.);
#3477=ORIENTED_EDGE('',*,*,#2775,.F.);
#3478=ORIENTED_EDGE('',*,*,#2799,.F.);
#3479=ORIENTED_EDGE('',*,*,#2782,.F.);
#3480=ORIENTED_EDGE('',*,*,#2764,.F.);
#3481=ORIENTED_EDGE('',*,*,#2749,.T.);
#3482=ORIENTED_EDGE('',*,*,#2802,.T.);
#3483=ORIENTED_EDGE('',*,*,#2715,.T.);
#3484=ORIENTED_EDGE('',*,*,#2803,.T.);
#3485=ORIENTED_EDGE('',*,*,#2787,.F.);
#3486=ORIENTED_EDGE('',*,*,#2798,.F.);
#3487=ORIENTED_EDGE('',*,*,#2774,.F.);
#3488=ORIENTED_EDGE('',*,*,#2789,.F.);
#3489=ORIENTED_EDGE('',*,*,#2725,.T.);
#3490=ORIENTED_EDGE('',*,*,#2756,.T.);
#3491=ORIENTED_EDGE('',*,*,#2794,.F.);
#3492=ORIENTED_EDGE('',*,*,#2788,.F.);
#3493=ORIENTED_EDGE('',*,*,#2766,.F.);
#3494=ORIENTED_EDGE('',*,*,#2759,.T.);
#3495=ORIENTED_EDGE('',*,*,#2802,.F.);
#3496=ORIENTED_EDGE('',*,*,#2748,.T.);
#3497=ORIENTED_EDGE('',*,*,#2754,.T.);
#3498=ORIENTED_EDGE('',*,*,#2804,.F.);
#3499=ORIENTED_EDGE('',*,*,#2804,.T.);
#3500=ORIENTED_EDGE('',*,*,#2805,.T.);
#3501=ORIENTED_EDGE('',*,*,#2803,.F.);
#3502=ORIENTED_EDGE('',*,*,#2805,.F.);
#3503=ORIENTED_EDGE('',*,*,#2781,.F.);
#3504=ORIENTED_EDGE('',*,*,#2801,.F.);
#3505=ORIENTED_EDGE('',*,*,#2792,.F.);
#3506=ORIENTED_EDGE('',*,*,#2795,.F.);
#3507=ORIENTED_EDGE('',*,*,#2806,.T.);
#3508=ORIENTED_EDGE('',*,*,#2807,.T.);
#3509=ORIENTED_EDGE('',*,*,#2808,.F.);
#3510=ORIENTED_EDGE('',*,*,#2807,.F.);
#3511=ORIENTED_EDGE('',*,*,#2806,.F.);
#3512=ORIENTED_EDGE('',*,*,#2809,.F.);
#3513=ORIENTED_EDGE('',*,*,#2810,.F.);
#3514=ORIENTED_EDGE('',*,*,#2811,.T.);
#3515=ORIENTED_EDGE('',*,*,#2812,.T.);
#3516=ORIENTED_EDGE('',*,*,#2811,.F.);
#3517=ORIENTED_EDGE('',*,*,#2812,.F.);
#3518=ORIENTED_EDGE('',*,*,#2813,.F.);
#3519=ORIENTED_EDGE('',*,*,#2814,.T.);
#3520=ORIENTED_EDGE('',*,*,#2815,.T.);
#3521=ORIENTED_EDGE('',*,*,#2814,.F.);
#3522=ORIENTED_EDGE('',*,*,#2815,.F.);
#3523=ORIENTED_EDGE('',*,*,#2816,.F.);
#3524=ORIENTED_EDGE('',*,*,#2817,.T.);
#3525=ORIENTED_EDGE('',*,*,#2818,.T.);
#3526=ORIENTED_EDGE('',*,*,#2817,.F.);
#3527=ORIENTED_EDGE('',*,*,#2818,.F.);
#3528=ORIENTED_EDGE('',*,*,#2819,.F.);
#3529=ORIENTED_EDGE('',*,*,#2820,.F.);
#3530=ORIENTED_EDGE('',*,*,#2821,.T.);
#3531=ORIENTED_EDGE('',*,*,#2822,.T.);
#3532=ORIENTED_EDGE('',*,*,#2821,.F.);
#3533=ORIENTED_EDGE('',*,*,#2822,.F.);
#3534=ORIENTED_EDGE('',*,*,#2823,.F.);
#3535=ORIENTED_EDGE('',*,*,#2823,.T.);
#3536=ORIENTED_EDGE('',*,*,#2824,.T.);
#3537=ORIENTED_EDGE('',*,*,#2809,.T.);
#3538=ORIENTED_EDGE('',*,*,#2824,.F.);
#3539=ORIENTED_EDGE('',*,*,#2819,.T.);
#3540=ORIENTED_EDGE('',*,*,#2825,.T.);
#3541=ORIENTED_EDGE('',*,*,#2826,.F.);
#3542=ORIENTED_EDGE('',*,*,#2825,.F.);
#3543=ORIENTED_EDGE('',*,*,#2827,.F.);
#3544=ORIENTED_EDGE('',*,*,#2828,.F.);
#3545=ORIENTED_EDGE('',*,*,#2829,.F.);
#3546=ORIENTED_EDGE('',*,*,#2830,.F.);
#3547=ORIENTED_EDGE('',*,*,#2831,.F.);
#3548=ORIENTED_EDGE('',*,*,#2832,.F.);
#3549=ORIENTED_EDGE('',*,*,#2833,.F.);
#3550=ORIENTED_EDGE('',*,*,#2834,.F.);
#3551=ORIENTED_EDGE('',*,*,#2835,.F.);
#3552=ORIENTED_EDGE('',*,*,#2836,.F.);
#3553=ORIENTED_EDGE('',*,*,#2837,.F.);
#3554=ORIENTED_EDGE('',*,*,#2838,.F.);
#3555=ORIENTED_EDGE('',*,*,#2837,.T.);
#3556=ORIENTED_EDGE('',*,*,#2839,.T.);
#3557=ORIENTED_EDGE('',*,*,#2828,.T.);
#3558=ORIENTED_EDGE('',*,*,#2840,.T.);
#3559=ORIENTED_EDGE('',*,*,#2841,.F.);
#3560=ORIENTED_EDGE('',*,*,#2842,.F.);
#3561=ORIENTED_EDGE('',*,*,#2843,.F.);
#3562=ORIENTED_EDGE('',*,*,#2844,.F.);
#3563=ORIENTED_EDGE('',*,*,#2845,.F.);
#3564=ORIENTED_EDGE('',*,*,#2846,.F.);
#3565=ORIENTED_EDGE('',*,*,#2845,.T.);
#3566=ORIENTED_EDGE('',*,*,#2847,.T.);
#3567=ORIENTED_EDGE('',*,*,#2831,.T.);
#3568=ORIENTED_EDGE('',*,*,#2848,.T.);
#3569=ORIENTED_EDGE('',*,*,#2849,.F.);
#3570=ORIENTED_EDGE('',*,*,#2850,.F.);
#3571=ORIENTED_EDGE('',*,*,#2851,.F.);
#3572=ORIENTED_EDGE('',*,*,#2850,.T.);
#3573=ORIENTED_EDGE('',*,*,#2852,.T.);
#3574=ORIENTED_EDGE('',*,*,#2834,.T.);
#3575=ORIENTED_EDGE('',*,*,#2853,.T.);
#3576=ORIENTED_EDGE('',*,*,#2836,.T.);
#3577=ORIENTED_EDGE('',*,*,#2854,.T.);
#3578=ORIENTED_EDGE('',*,*,#2851,.T.);
#3579=ORIENTED_EDGE('',*,*,#2855,.T.);
#3580=ORIENTED_EDGE('',*,*,#2856,.F.);
#3581=ORIENTED_EDGE('',*,*,#2857,.F.);
#3582=ORIENTED_EDGE('',*,*,#2858,.F.);
#3583=ORIENTED_EDGE('',*,*,#2842,.T.);
#3584=ORIENTED_EDGE('',*,*,#2859,.T.);
#3585=ORIENTED_EDGE('',*,*,#2857,.T.);
#3586=ORIENTED_EDGE('',*,*,#2860,.T.);
#3587=ORIENTED_EDGE('',*,*,#2849,.T.);
#3588=ORIENTED_EDGE('',*,*,#2861,.T.);
#3589=ORIENTED_EDGE('',*,*,#2858,.T.);
#3590=ORIENTED_EDGE('',*,*,#2862,.T.);
#3591=ORIENTED_EDGE('',*,*,#2856,.T.);
#3592=ORIENTED_EDGE('',*,*,#2863,.T.);
#3593=ORIENTED_EDGE('',*,*,#2846,.T.);
#3594=ORIENTED_EDGE('',*,*,#2864,.T.);
#3595=ORIENTED_EDGE('',*,*,#2844,.T.);
#3596=ORIENTED_EDGE('',*,*,#2865,.T.);
#3597=ORIENTED_EDGE('',*,*,#2838,.T.);
#3598=ORIENTED_EDGE('',*,*,#2866,.T.);
#3599=ORIENTED_EDGE('',*,*,#2830,.T.);
#3600=ORIENTED_EDGE('',*,*,#2867,.T.);
#3601=ORIENTED_EDGE('',*,*,#2843,.T.);
#3602=ORIENTED_EDGE('',*,*,#2868,.T.);
#3603=ORIENTED_EDGE('',*,*,#2841,.T.);
#3604=ORIENTED_EDGE('',*,*,#2869,.T.);
#3605=ORIENTED_EDGE('',*,*,#2835,.T.);
#3606=ORIENTED_EDGE('',*,*,#2870,.T.);
#3607=ORIENTED_EDGE('',*,*,#2833,.T.);
#3608=ORIENTED_EDGE('',*,*,#2871,.T.);
#3609=ORIENTED_EDGE('',*,*,#2829,.T.);
#3610=ORIENTED_EDGE('',*,*,#2872,.T.);
#3611=ORIENTED_EDGE('',*,*,#2827,.T.);
#3612=ORIENTED_EDGE('',*,*,#2873,.T.);
#3613=ORIENTED_EDGE('',*,*,#2832,.T.);
#3614=ORIENTED_EDGE('',*,*,#2874,.T.);
#3615=ORIENTED_EDGE('',*,*,#2847,.F.);
#3616=ORIENTED_EDGE('',*,*,#2866,.F.);
#3617=ORIENTED_EDGE('',*,*,#2840,.F.);
#3618=ORIENTED_EDGE('',*,*,#2874,.F.);
#3619=ORIENTED_EDGE('',*,*,#2808,.T.);
#3620=ORIENTED_EDGE('',*,*,#2875,.T.);
#3621=ORIENTED_EDGE('',*,*,#2876,.T.);
#3622=ORIENTED_EDGE('',*,*,#2853,.F.);
#3623=ORIENTED_EDGE('',*,*,#2872,.F.);
#3624=ORIENTED_EDGE('',*,*,#2839,.F.);
#3625=ORIENTED_EDGE('',*,*,#2855,.F.);
#3626=ORIENTED_EDGE('',*,*,#2854,.F.);
#3627=ORIENTED_EDGE('',*,*,#2865,.F.);
#3628=ORIENTED_EDGE('',*,*,#2863,.F.);
#3629=ORIENTED_EDGE('',*,*,#2861,.F.);
#3630=ORIENTED_EDGE('',*,*,#2810,.T.);
#3631=ORIENTED_EDGE('',*,*,#2813,.T.);
#3632=ORIENTED_EDGE('',*,*,#2860,.F.);
#3633=ORIENTED_EDGE('',*,*,#2864,.F.);
#3634=ORIENTED_EDGE('',*,*,#2848,.F.);
#3635=ORIENTED_EDGE('',*,*,#2868,.F.);
#3636=ORIENTED_EDGE('',*,*,#2859,.F.);
#3637=ORIENTED_EDGE('',*,*,#2870,.F.);
#3638=ORIENTED_EDGE('',*,*,#2852,.F.);
#3639=ORIENTED_EDGE('',*,*,#2862,.F.);
#3640=ORIENTED_EDGE('',*,*,#2816,.T.);
#3641=ORIENTED_EDGE('',*,*,#2820,.T.);
#3642=ORIENTED_EDGE('',*,*,#2867,.F.);
#3643=ORIENTED_EDGE('',*,*,#2873,.F.);
#3644=ORIENTED_EDGE('',*,*,#2871,.F.);
#3645=ORIENTED_EDGE('',*,*,#2869,.F.);
#3646=ORIENTED_EDGE('',*,*,#2876,.F.);
#3647=ORIENTED_EDGE('',*,*,#2877,.T.);
#3648=ORIENTED_EDGE('',*,*,#2878,.T.);
#3649=ORIENTED_EDGE('',*,*,#2877,.F.);
#3650=ORIENTED_EDGE('',*,*,#2878,.F.);
#3651=ORIENTED_EDGE('',*,*,#2826,.T.);
#3652=ORIENTED_EDGE('',*,*,#2875,.F.);
#3653=ORIENTED_EDGE('',*,*,#2879,.T.);
#3654=ORIENTED_EDGE('',*,*,#2880,.T.);
#3655=ORIENTED_EDGE('',*,*,#2879,.F.);
#3656=ORIENTED_EDGE('',*,*,#2880,.F.);
#3657=ORIENTED_EDGE('',*,*,#2881,.T.);
#3658=ORIENTED_EDGE('',*,*,#2882,.T.);
#3659=ORIENTED_EDGE('',*,*,#2883,.F.);
#3660=ORIENTED_EDGE('',*,*,#2882,.F.);
#3661=ORIENTED_EDGE('',*,*,#2884,.T.);
#3662=ORIENTED_EDGE('',*,*,#2885,.T.);
#3663=ORIENTED_EDGE('',*,*,#2886,.F.);
#3664=ORIENTED_EDGE('',*,*,#2885,.F.);
#3665=ORIENTED_EDGE('',*,*,#2884,.F.);
#3666=ORIENTED_EDGE('',*,*,#2887,.T.);
#3667=ORIENTED_EDGE('',*,*,#2888,.T.);
#3668=ORIENTED_EDGE('',*,*,#2889,.T.);
#3669=ORIENTED_EDGE('',*,*,#2887,.F.);
#3670=ORIENTED_EDGE('',*,*,#2889,.F.);
#3671=ORIENTED_EDGE('',*,*,#2890,.T.);
#3672=ORIENTED_EDGE('',*,*,#2891,.T.);
#3673=ORIENTED_EDGE('',*,*,#2890,.F.);
#3674=ORIENTED_EDGE('',*,*,#2888,.F.);
#3675=ORIENTED_EDGE('',*,*,#2892,.F.);
#3676=ORIENTED_EDGE('',*,*,#2893,.T.);
#3677=ORIENTED_EDGE('',*,*,#2883,.T.);
#3678=ORIENTED_EDGE('',*,*,#2893,.F.);
#3679=ORIENTED_EDGE('',*,*,#2881,.F.);
#3680=ORIENTED_EDGE('',*,*,#2894,.T.);
#3681=ORIENTED_EDGE('',*,*,#2895,.T.);
#3682=ORIENTED_EDGE('',*,*,#2894,.F.);
#3683=ORIENTED_EDGE('',*,*,#2895,.F.);
#3684=ORIENTED_EDGE('',*,*,#2886,.T.);
#3685=ORIENTED_EDGE('',*,*,#2892,.T.);
#3686=ORIENTED_EDGE('',*,*,#2891,.F.);
#3687=ORIENTED_EDGE('',*,*,#2896,.T.);
#3688=ORIENTED_EDGE('',*,*,#2896,.F.);
#3689=ORIENTED_EDGE('',*,*,#2897,.T.);
#3690=ORIENTED_EDGE('',*,*,#2898,.T.);
#3691=ORIENTED_EDGE('',*,*,#2899,.F.);
#3692=ORIENTED_EDGE('',*,*,#2898,.F.);
#3693=ORIENTED_EDGE('',*,*,#2900,.F.);
#3694=ORIENTED_EDGE('',*,*,#2901,.T.);
#3695=ORIENTED_EDGE('',*,*,#2902,.T.);
#3696=ORIENTED_EDGE('',*,*,#2901,.F.);
#3697=ORIENTED_EDGE('',*,*,#2900,.T.);
#3698=ORIENTED_EDGE('',*,*,#2903,.T.);
#3699=ORIENTED_EDGE('',*,*,#2904,.F.);
#3700=ORIENTED_EDGE('',*,*,#2903,.F.);
#3701=ORIENTED_EDGE('',*,*,#2905,.F.);
#3702=ORIENTED_EDGE('',*,*,#2906,.T.);
#3703=ORIENTED_EDGE('',*,*,#2904,.T.);
#3704=ORIENTED_EDGE('',*,*,#2906,.F.);
#3705=ORIENTED_EDGE('',*,*,#2907,.F.);
#3706=ORIENTED_EDGE('',*,*,#2908,.F.);
#3707=ORIENTED_EDGE('',*,*,#2909,.T.);
#3708=ORIENTED_EDGE('',*,*,#2910,.T.);
#3709=ORIENTED_EDGE('',*,*,#2909,.F.);
#3710=ORIENTED_EDGE('',*,*,#2897,.F.);
#3711=ORIENTED_EDGE('',*,*,#2911,.T.);
#3712=ORIENTED_EDGE('',*,*,#2907,.T.);
#3713=ORIENTED_EDGE('',*,*,#2908,.T.);
#3714=ORIENTED_EDGE('',*,*,#2911,.F.);
#3715=ORIENTED_EDGE('',*,*,#2910,.F.);
#3716=ORIENTED_EDGE('',*,*,#2905,.T.);
#3717=ORIENTED_EDGE('',*,*,#2899,.T.);
#3718=ORIENTED_EDGE('',*,*,#2902,.F.);
#3719=ORIENTED_EDGE('',*,*,#2912,.T.);
#3720=ORIENTED_EDGE('',*,*,#2912,.F.);
#3721=ORIENTED_EDGE('',*,*,#2913,.T.);
#3722=ORIENTED_EDGE('',*,*,#2913,.F.);
#3723=ORIENTED_EDGE('',*,*,#2914,.T.);
#3724=ORIENTED_EDGE('',*,*,#2914,.F.);
#3725=ORIENTED_EDGE('',*,*,#2915,.T.);
#3726=ORIENTED_EDGE('',*,*,#2915,.F.);
#3727=ORIENTED_EDGE('',*,*,#2916,.T.);
#3728=ORIENTED_EDGE('',*,*,#2916,.F.);
#3729=ORIENTED_EDGE('',*,*,#2917,.T.);
#3730=ORIENTED_EDGE('',*,*,#2917,.F.);
#3731=ORIENTED_EDGE('',*,*,#2918,.T.);
#3732=ORIENTED_EDGE('',*,*,#2918,.F.);
#3733=ORIENTED_EDGE('',*,*,#2919,.T.);
#3734=ORIENTED_EDGE('',*,*,#2919,.F.);
#3735=ORIENTED_EDGE('',*,*,#2920,.T.);
#3736=ORIENTED_EDGE('',*,*,#2920,.F.);
#3737=ORIENTED_EDGE('',*,*,#2921,.F.);
#3738=ORIENTED_EDGE('',*,*,#2922,.T.);
#3739=ORIENTED_EDGE('',*,*,#2923,.T.);
#3740=ORIENTED_EDGE('',*,*,#2922,.F.);
#3741=ORIENTED_EDGE('',*,*,#2924,.T.);
#3742=ORIENTED_EDGE('',*,*,#2924,.F.);
#3743=ORIENTED_EDGE('',*,*,#2925,.T.);
#3744=ORIENTED_EDGE('',*,*,#2926,.F.);
#3745=ORIENTED_EDGE('',*,*,#2923,.F.);
#3746=ORIENTED_EDGE('',*,*,#2926,.T.);
#3747=ORIENTED_EDGE('',*,*,#2921,.T.);
#3748=ORIENTED_EDGE('',*,*,#2925,.F.);
#3749=ORIENTED_EDGE('',*,*,#2927,.F.);
#3750=ORIENTED_EDGE('',*,*,#2928,.T.);
#3751=ORIENTED_EDGE('',*,*,#2929,.T.);
#3752=ORIENTED_EDGE('',*,*,#2928,.F.);
#3753=ORIENTED_EDGE('',*,*,#2930,.T.);
#3754=ORIENTED_EDGE('',*,*,#2930,.F.);
#3755=ORIENTED_EDGE('',*,*,#2931,.T.);
#3756=ORIENTED_EDGE('',*,*,#2932,.F.);
#3757=ORIENTED_EDGE('',*,*,#2929,.F.);
#3758=ORIENTED_EDGE('',*,*,#2932,.T.);
#3759=ORIENTED_EDGE('',*,*,#2927,.T.);
#3760=ORIENTED_EDGE('',*,*,#2931,.F.);
#3761=ORIENTED_EDGE('',*,*,#2933,.F.);
#3762=ORIENTED_EDGE('',*,*,#2934,.T.);
#3763=ORIENTED_EDGE('',*,*,#2935,.T.);
#3764=ORIENTED_EDGE('',*,*,#2934,.F.);
#3765=ORIENTED_EDGE('',*,*,#2936,.T.);
#3766=ORIENTED_EDGE('',*,*,#2936,.F.);
#3767=ORIENTED_EDGE('',*,*,#2937,.T.);
#3768=ORIENTED_EDGE('',*,*,#2938,.F.);
#3769=ORIENTED_EDGE('',*,*,#2935,.F.);
#3770=ORIENTED_EDGE('',*,*,#2938,.T.);
#3771=ORIENTED_EDGE('',*,*,#2933,.T.);
#3772=ORIENTED_EDGE('',*,*,#2937,.F.);
#3773=ORIENTED_EDGE('',*,*,#2939,.F.);
#3774=ORIENTED_EDGE('',*,*,#2940,.T.);
#3775=ORIENTED_EDGE('',*,*,#2941,.T.);
#3776=ORIENTED_EDGE('',*,*,#2940,.F.);
#3777=ORIENTED_EDGE('',*,*,#2942,.T.);
#3778=ORIENTED_EDGE('',*,*,#2942,.F.);
#3779=ORIENTED_EDGE('',*,*,#2943,.T.);
#3780=ORIENTED_EDGE('',*,*,#2944,.F.);
#3781=ORIENTED_EDGE('',*,*,#2941,.F.);
#3782=ORIENTED_EDGE('',*,*,#2944,.T.);
#3783=ORIENTED_EDGE('',*,*,#2939,.T.);
#3784=ORIENTED_EDGE('',*,*,#2943,.F.);
#3785=ORIENTED_EDGE('',*,*,#2945,.F.);
#3786=ORIENTED_EDGE('',*,*,#2946,.T.);
#3787=ORIENTED_EDGE('',*,*,#2947,.T.);
#3788=ORIENTED_EDGE('',*,*,#2946,.F.);
#3789=ORIENTED_EDGE('',*,*,#2948,.T.);
#3790=ORIENTED_EDGE('',*,*,#2948,.F.);
#3791=ORIENTED_EDGE('',*,*,#2949,.T.);
#3792=ORIENTED_EDGE('',*,*,#2950,.F.);
#3793=ORIENTED_EDGE('',*,*,#2947,.F.);
#3794=ORIENTED_EDGE('',*,*,#2950,.T.);
#3795=ORIENTED_EDGE('',*,*,#2945,.T.);
#3796=ORIENTED_EDGE('',*,*,#2949,.F.);
#3797=ORIENTED_EDGE('',*,*,#2951,.F.);
#3798=ORIENTED_EDGE('',*,*,#2952,.T.);
#3799=ORIENTED_EDGE('',*,*,#2953,.T.);
#3800=ORIENTED_EDGE('',*,*,#2952,.F.);
#3801=ORIENTED_EDGE('',*,*,#2954,.T.);
#3802=ORIENTED_EDGE('',*,*,#2954,.F.);
#3803=ORIENTED_EDGE('',*,*,#2955,.T.);
#3804=ORIENTED_EDGE('',*,*,#2956,.F.);
#3805=ORIENTED_EDGE('',*,*,#2953,.F.);
#3806=ORIENTED_EDGE('',*,*,#2956,.T.);
#3807=ORIENTED_EDGE('',*,*,#2951,.T.);
#3808=ORIENTED_EDGE('',*,*,#2955,.F.);
#3809=ORIENTED_EDGE('',*,*,#2957,.F.);
#3810=ORIENTED_EDGE('',*,*,#2958,.T.);
#3811=ORIENTED_EDGE('',*,*,#2959,.T.);
#3812=ORIENTED_EDGE('',*,*,#2958,.F.);
#3813=ORIENTED_EDGE('',*,*,#2960,.T.);
#3814=ORIENTED_EDGE('',*,*,#2960,.F.);
#3815=ORIENTED_EDGE('',*,*,#2961,.T.);
#3816=ORIENTED_EDGE('',*,*,#2962,.F.);
#3817=ORIENTED_EDGE('',*,*,#2959,.F.);
#3818=ORIENTED_EDGE('',*,*,#2962,.T.);
#3819=ORIENTED_EDGE('',*,*,#2957,.T.);
#3820=ORIENTED_EDGE('',*,*,#2961,.F.);
#3821=ORIENTED_EDGE('',*,*,#2963,.F.);
#3822=ORIENTED_EDGE('',*,*,#2964,.T.);
#3823=ORIENTED_EDGE('',*,*,#2965,.T.);
#3824=ORIENTED_EDGE('',*,*,#2964,.F.);
#3825=ORIENTED_EDGE('',*,*,#2966,.T.);
#3826=ORIENTED_EDGE('',*,*,#2966,.F.);
#3827=ORIENTED_EDGE('',*,*,#2967,.T.);
#3828=ORIENTED_EDGE('',*,*,#2968,.F.);
#3829=ORIENTED_EDGE('',*,*,#2965,.F.);
#3830=ORIENTED_EDGE('',*,*,#2968,.T.);
#3831=ORIENTED_EDGE('',*,*,#2963,.T.);
#3832=ORIENTED_EDGE('',*,*,#2967,.F.);
#3833=ORIENTED_EDGE('',*,*,#2969,.F.);
#3834=ORIENTED_EDGE('',*,*,#2970,.T.);
#3835=ORIENTED_EDGE('',*,*,#2971,.T.);
#3836=ORIENTED_EDGE('',*,*,#2970,.F.);
#3837=ORIENTED_EDGE('',*,*,#2972,.T.);
#3838=ORIENTED_EDGE('',*,*,#2972,.F.);
#3839=ORIENTED_EDGE('',*,*,#2973,.T.);
#3840=ORIENTED_EDGE('',*,*,#2974,.F.);
#3841=ORIENTED_EDGE('',*,*,#2971,.F.);
#3842=ORIENTED_EDGE('',*,*,#2974,.T.);
#3843=ORIENTED_EDGE('',*,*,#2969,.T.);
#3844=ORIENTED_EDGE('',*,*,#2973,.F.);
#3845=ORIENTED_EDGE('',*,*,#2975,.F.);
#3846=ORIENTED_EDGE('',*,*,#2976,.T.);
#3847=ORIENTED_EDGE('',*,*,#2977,.T.);
#3848=ORIENTED_EDGE('',*,*,#2976,.F.);
#3849=ORIENTED_EDGE('',*,*,#2978,.T.);
#3850=ORIENTED_EDGE('',*,*,#2978,.F.);
#3851=ORIENTED_EDGE('',*,*,#2979,.T.);
#3852=ORIENTED_EDGE('',*,*,#2980,.F.);
#3853=ORIENTED_EDGE('',*,*,#2977,.F.);
#3854=ORIENTED_EDGE('',*,*,#2980,.T.);
#3855=ORIENTED_EDGE('',*,*,#2975,.T.);
#3856=ORIENTED_EDGE('',*,*,#2979,.F.);
#3857=ORIENTED_EDGE('',*,*,#2981,.T.);
#3858=ORIENTED_EDGE('',*,*,#2982,.T.);
#3859=ORIENTED_EDGE('',*,*,#2983,.F.);
#3860=ORIENTED_EDGE('',*,*,#2982,.F.);
#3861=ORIENTED_EDGE('',*,*,#2984,.T.);
#3862=ORIENTED_EDGE('',*,*,#2985,.T.);
#3863=ORIENTED_EDGE('',*,*,#2986,.F.);
#3864=ORIENTED_EDGE('',*,*,#2985,.F.);
#3865=ORIENTED_EDGE('',*,*,#2984,.F.);
#3866=ORIENTED_EDGE('',*,*,#2983,.T.);
#3867=ORIENTED_EDGE('',*,*,#2986,.T.);
#3868=ORIENTED_EDGE('',*,*,#2981,.F.);
#3869=ORIENTED_EDGE('',*,*,#2987,.F.);
#3870=ORIENTED_EDGE('',*,*,#2988,.T.);
#3871=ORIENTED_EDGE('',*,*,#2989,.T.);
#3872=ORIENTED_EDGE('',*,*,#2988,.F.);
#3873=ORIENTED_EDGE('',*,*,#2990,.T.);
#3874=ORIENTED_EDGE('',*,*,#2990,.F.);
#3875=ORIENTED_EDGE('',*,*,#2991,.T.);
#3876=ORIENTED_EDGE('',*,*,#2992,.F.);
#3877=ORIENTED_EDGE('',*,*,#2989,.F.);
#3878=ORIENTED_EDGE('',*,*,#2992,.T.);
#3879=ORIENTED_EDGE('',*,*,#2987,.T.);
#3880=ORIENTED_EDGE('',*,*,#2991,.F.);
#3881=ORIENTED_EDGE('',*,*,#2993,.F.);
#3882=ORIENTED_EDGE('',*,*,#2994,.T.);
#3883=ORIENTED_EDGE('',*,*,#2995,.T.);
#3884=ORIENTED_EDGE('',*,*,#2994,.F.);
#3885=ORIENTED_EDGE('',*,*,#2996,.T.);
#3886=ORIENTED_EDGE('',*,*,#2996,.F.);
#3887=ORIENTED_EDGE('',*,*,#2997,.T.);
#3888=ORIENTED_EDGE('',*,*,#2998,.F.);
#3889=ORIENTED_EDGE('',*,*,#2995,.F.);
#3890=ORIENTED_EDGE('',*,*,#2998,.T.);
#3891=ORIENTED_EDGE('',*,*,#2993,.T.);
#3892=ORIENTED_EDGE('',*,*,#2997,.F.);
#3893=ORIENTED_EDGE('',*,*,#2999,.T.);
#3894=ORIENTED_EDGE('',*,*,#2999,.F.);
#3895=ORIENTED_EDGE('',*,*,#3000,.T.);
#3896=ORIENTED_EDGE('',*,*,#3000,.F.);
#3897=ORIENTED_EDGE('',*,*,#3001,.T.);
#3898=ORIENTED_EDGE('',*,*,#3002,.T.);
#3899=ORIENTED_EDGE('',*,*,#3003,.T.);
#3900=ORIENTED_EDGE('',*,*,#3004,.T.);
#3901=ORIENTED_EDGE('',*,*,#3002,.F.);
#3902=ORIENTED_EDGE('',*,*,#3005,.T.);
#3903=ORIENTED_EDGE('',*,*,#3006,.T.);
#3904=ORIENTED_EDGE('',*,*,#3007,.T.);
#3905=ORIENTED_EDGE('',*,*,#3006,.F.);
#3906=ORIENTED_EDGE('',*,*,#3008,.T.);
#3907=ORIENTED_EDGE('',*,*,#3009,.F.);
#3908=ORIENTED_EDGE('',*,*,#3010,.F.);
#3909=ORIENTED_EDGE('',*,*,#3011,.T.);
#3910=ORIENTED_EDGE('',*,*,#3008,.F.);
#3911=ORIENTED_EDGE('',*,*,#3005,.F.);
#3912=ORIENTED_EDGE('',*,*,#3011,.F.);
#3913=ORIENTED_EDGE('',*,*,#3012,.F.);
#3914=ORIENTED_EDGE('',*,*,#3013,.T.);
#3915=ORIENTED_EDGE('',*,*,#3009,.T.);
#3916=ORIENTED_EDGE('',*,*,#3010,.T.);
#3917=ORIENTED_EDGE('',*,*,#3013,.F.);
#3918=ORIENTED_EDGE('',*,*,#3014,.T.);
#3919=ORIENTED_EDGE('',*,*,#3015,.T.);
#3920=ORIENTED_EDGE('',*,*,#3016,.F.);
#3921=ORIENTED_EDGE('',*,*,#3015,.F.);
#3922=ORIENTED_EDGE('',*,*,#3004,.F.);
#3923=ORIENTED_EDGE('',*,*,#3017,.T.);
#3924=ORIENTED_EDGE('',*,*,#3016,.T.);
#3925=ORIENTED_EDGE('',*,*,#3017,.F.);
#3926=ORIENTED_EDGE('',*,*,#3003,.F.);
#3927=ORIENTED_EDGE('',*,*,#3007,.F.);
#3928=ORIENTED_EDGE('',*,*,#3001,.F.);
#3929=ORIENTED_EDGE('',*,*,#3012,.T.);
#3930=ORIENTED_EDGE('',*,*,#3014,.F.);
#3931=ORIENTED_EDGE('',*,*,#3018,.T.);
#3932=ORIENTED_EDGE('',*,*,#3019,.T.);
#3933=ORIENTED_EDGE('',*,*,#3020,.T.);
#3934=ORIENTED_EDGE('',*,*,#3019,.F.);
#3935=ORIENTED_EDGE('',*,*,#3021,.T.);
#3936=ORIENTED_EDGE('',*,*,#3022,.T.);
#3937=ORIENTED_EDGE('',*,*,#3023,.T.);
#3938=ORIENTED_EDGE('',*,*,#3022,.F.);
#3939=ORIENTED_EDGE('',*,*,#3024,.F.);
#3940=ORIENTED_EDGE('',*,*,#3025,.F.);
#3941=ORIENTED_EDGE('',*,*,#3026,.T.);
#3942=ORIENTED_EDGE('',*,*,#3023,.F.);
#3943=ORIENTED_EDGE('',*,*,#3026,.F.);
#3944=ORIENTED_EDGE('',*,*,#3027,.F.);
#3945=ORIENTED_EDGE('',*,*,#3028,.T.);
#3946=ORIENTED_EDGE('',*,*,#3024,.T.);
#3947=ORIENTED_EDGE('',*,*,#3025,.T.);
#3948=ORIENTED_EDGE('',*,*,#3028,.F.);
#3949=ORIENTED_EDGE('',*,*,#3029,.T.);
#3950=ORIENTED_EDGE('',*,*,#3030,.T.);
#3951=ORIENTED_EDGE('',*,*,#3031,.F.);
#3952=ORIENTED_EDGE('',*,*,#3030,.F.);
#3953=ORIENTED_EDGE('',*,*,#3018,.F.);
#3954=ORIENTED_EDGE('',*,*,#3032,.T.);
#3955=ORIENTED_EDGE('',*,*,#3031,.T.);
#3956=ORIENTED_EDGE('',*,*,#3032,.F.);
#3957=ORIENTED_EDGE('',*,*,#3029,.F.);
#3958=ORIENTED_EDGE('',*,*,#3027,.T.);
#3959=ORIENTED_EDGE('',*,*,#3020,.F.);
#3960=ORIENTED_EDGE('',*,*,#3021,.F.);
#3961=ORIENTED_EDGE('',*,*,#3033,.F.);
#3962=ORIENTED_EDGE('',*,*,#3034,.T.);
#3963=ORIENTED_EDGE('',*,*,#3035,.F.);
#3964=ORIENTED_EDGE('',*,*,#3034,.F.);
#3965=ORIENTED_EDGE('',*,*,#3036,.T.);
#3966=ORIENTED_EDGE('',*,*,#3037,.T.);
#3967=ORIENTED_EDGE('',*,*,#3038,.T.);
#3968=ORIENTED_EDGE('',*,*,#3037,.F.);
#3969=ORIENTED_EDGE('',*,*,#3038,.F.);
#3970=ORIENTED_EDGE('',*,*,#3039,.T.);
#3971=ORIENTED_EDGE('',*,*,#3040,.T.);
#3972=ORIENTED_EDGE('',*,*,#3041,.T.);
#3973=ORIENTED_EDGE('',*,*,#3042,.T.);
#3974=ORIENTED_EDGE('',*,*,#3043,.T.);
#3975=ORIENTED_EDGE('',*,*,#3044,.T.);
#3976=ORIENTED_EDGE('',*,*,#3045,.F.);
#3977=ORIENTED_EDGE('',*,*,#3046,.T.);
#3978=ORIENTED_EDGE('',*,*,#3036,.F.);
#3979=ORIENTED_EDGE('',*,*,#3046,.F.);
#3980=ORIENTED_EDGE('',*,*,#3047,.F.);
#3981=ORIENTED_EDGE('',*,*,#3048,.F.);
#3982=ORIENTED_EDGE('',*,*,#3049,.T.);
#3983=ORIENTED_EDGE('',*,*,#3049,.F.);
#3984=ORIENTED_EDGE('',*,*,#3050,.F.);
#3985=ORIENTED_EDGE('',*,*,#3051,.T.);
#3986=ORIENTED_EDGE('',*,*,#3051,.F.);
#3987=ORIENTED_EDGE('',*,*,#3052,.F.);
#3988=ORIENTED_EDGE('',*,*,#3053,.T.);
#3989=ORIENTED_EDGE('',*,*,#3053,.F.);
#3990=ORIENTED_EDGE('',*,*,#3054,.F.);
#3991=ORIENTED_EDGE('',*,*,#3055,.T.);
#3992=ORIENTED_EDGE('',*,*,#3055,.F.);
#3993=ORIENTED_EDGE('',*,*,#3056,.F.);
#3994=ORIENTED_EDGE('',*,*,#3057,.T.);
#3995=ORIENTED_EDGE('',*,*,#3057,.F.);
#3996=ORIENTED_EDGE('',*,*,#3058,.F.);
#3997=ORIENTED_EDGE('',*,*,#3047,.T.);
#3998=ORIENTED_EDGE('',*,*,#3039,.F.);
#3999=ORIENTED_EDGE('',*,*,#3059,.T.);
#4000=ORIENTED_EDGE('',*,*,#3048,.T.);
#4001=ORIENTED_EDGE('',*,*,#3060,.F.);
#4002=ORIENTED_EDGE('',*,*,#3044,.F.);
#4003=ORIENTED_EDGE('',*,*,#3061,.T.);
#4004=ORIENTED_EDGE('',*,*,#3050,.T.);
#4005=ORIENTED_EDGE('',*,*,#3059,.F.);
#4006=ORIENTED_EDGE('',*,*,#3043,.F.);
#4007=ORIENTED_EDGE('',*,*,#3062,.T.);
#4008=ORIENTED_EDGE('',*,*,#3052,.T.);
#4009=ORIENTED_EDGE('',*,*,#3061,.F.);
#4010=ORIENTED_EDGE('',*,*,#3042,.F.);
#4011=ORIENTED_EDGE('',*,*,#3063,.T.);
#4012=ORIENTED_EDGE('',*,*,#3054,.T.);
#4013=ORIENTED_EDGE('',*,*,#3062,.F.);
#4014=ORIENTED_EDGE('',*,*,#3041,.F.);
#4015=ORIENTED_EDGE('',*,*,#3064,.T.);
#4016=ORIENTED_EDGE('',*,*,#3056,.T.);
#4017=ORIENTED_EDGE('',*,*,#3063,.F.);
#4018=ORIENTED_EDGE('',*,*,#3040,.F.);
#4019=ORIENTED_EDGE('',*,*,#3060,.T.);
#4020=ORIENTED_EDGE('',*,*,#3058,.T.);
#4021=ORIENTED_EDGE('',*,*,#3064,.F.);
#4022=ORIENTED_EDGE('',*,*,#3033,.T.);
#4023=ORIENTED_EDGE('',*,*,#3065,.T.);
#4024=ORIENTED_EDGE('',*,*,#3066,.T.);
#4025=ORIENTED_EDGE('',*,*,#3065,.F.);
#4026=ORIENTED_EDGE('',*,*,#3035,.T.);
#4027=ORIENTED_EDGE('',*,*,#3045,.T.);
#4028=ORIENTED_EDGE('',*,*,#3066,.F.);
#4029=ORIENTED_EDGE('',*,*,#3067,.F.);
#4030=ORIENTED_EDGE('',*,*,#3068,.T.);
#4031=ORIENTED_EDGE('',*,*,#3069,.T.);
#4032=ORIENTED_EDGE('',*,*,#3068,.F.);
#4033=ORIENTED_EDGE('',*,*,#3069,.F.);
#4034=ORIENTED_EDGE('',*,*,#3070,.F.);
#4035=ORIENTED_EDGE('',*,*,#3071,.T.);
#4036=ORIENTED_EDGE('',*,*,#3072,.T.);
#4037=ORIENTED_EDGE('',*,*,#3071,.F.);
#4038=ORIENTED_EDGE('',*,*,#3072,.F.);
#4039=ORIENTED_EDGE('',*,*,#3073,.F.);
#4040=ORIENTED_EDGE('',*,*,#3067,.T.);
#4041=ORIENTED_EDGE('',*,*,#3073,.T.);
#4042=ORIENTED_EDGE('',*,*,#3074,.T.);
#4043=ORIENTED_EDGE('',*,*,#3075,.T.);
#4044=ORIENTED_EDGE('',*,*,#3074,.F.);
#4045=ORIENTED_EDGE('',*,*,#3075,.F.);
#4046=ORIENTED_EDGE('',*,*,#3070,.T.);
#4047=ORIENTED_EDGE('',*,*,#3076,.T.);
#4048=ORIENTED_EDGE('',*,*,#3077,.F.);
#4049=ORIENTED_EDGE('',*,*,#3078,.T.);
#4050=ORIENTED_EDGE('',*,*,#3076,.F.);
#4051=ORIENTED_EDGE('',*,*,#3078,.F.);
#4052=ORIENTED_EDGE('',*,*,#3077,.T.);
#4053=ORIENTED_EDGE('',*,*,#3079,.F.);
#4054=ORIENTED_EDGE('',*,*,#3080,.T.);
#4055=ORIENTED_EDGE('',*,*,#3081,.T.);
#4056=ORIENTED_EDGE('',*,*,#3080,.F.);
#4057=ORIENTED_EDGE('',*,*,#3081,.F.);
#4058=ORIENTED_EDGE('',*,*,#3082,.F.);
#4059=ORIENTED_EDGE('',*,*,#3083,.T.);
#4060=ORIENTED_EDGE('',*,*,#3084,.T.);
#4061=ORIENTED_EDGE('',*,*,#3083,.F.);
#4062=ORIENTED_EDGE('',*,*,#3084,.F.);
#4063=ORIENTED_EDGE('',*,*,#3085,.T.);
#4064=ORIENTED_EDGE('',*,*,#3079,.T.);
#4065=ORIENTED_EDGE('',*,*,#3086,.F.);
#4066=ORIENTED_EDGE('',*,*,#3087,.T.);
#4067=ORIENTED_EDGE('',*,*,#3085,.F.);
#4068=ORIENTED_EDGE('',*,*,#3087,.F.);
#4069=ORIENTED_EDGE('',*,*,#3086,.T.);
#4070=ORIENTED_EDGE('',*,*,#3082,.T.);
#4071=ORIENTED_EDGE('',*,*,#3088,.F.);
#4072=ORIENTED_EDGE('',*,*,#3089,.T.);
#4073=ORIENTED_EDGE('',*,*,#3090,.T.);
#4074=ORIENTED_EDGE('',*,*,#3089,.F.);
#4075=ORIENTED_EDGE('',*,*,#3091,.F.);
#4076=ORIENTED_EDGE('',*,*,#3092,.T.);
#4077=ORIENTED_EDGE('',*,*,#3093,.T.);
#4078=ORIENTED_EDGE('',*,*,#3092,.F.);
#4079=ORIENTED_EDGE('',*,*,#3094,.F.);
#4080=ORIENTED_EDGE('',*,*,#3095,.F.);
#4081=ORIENTED_EDGE('',*,*,#3096,.T.);
#4082=ORIENTED_EDGE('',*,*,#3091,.T.);
#4083=ORIENTED_EDGE('',*,*,#3096,.F.);
#4084=ORIENTED_EDGE('',*,*,#3094,.T.);
#4085=ORIENTED_EDGE('',*,*,#3095,.T.);
#4086=ORIENTED_EDGE('',*,*,#3097,.T.);
#4087=ORIENTED_EDGE('',*,*,#3098,.F.);
#4088=ORIENTED_EDGE('',*,*,#3097,.F.);
#4089=ORIENTED_EDGE('',*,*,#3090,.F.);
#4090=ORIENTED_EDGE('',*,*,#3099,.T.);
#4091=ORIENTED_EDGE('',*,*,#3100,.T.);
#4092=ORIENTED_EDGE('',*,*,#3099,.F.);
#4093=ORIENTED_EDGE('',*,*,#3101,.F.);
#4094=ORIENTED_EDGE('',*,*,#3102,.T.);
#4095=ORIENTED_EDGE('',*,*,#3088,.T.);
#4096=ORIENTED_EDGE('',*,*,#3102,.F.);
#4097=ORIENTED_EDGE('',*,*,#3101,.T.);
#4098=ORIENTED_EDGE('',*,*,#3093,.F.);
#4099=ORIENTED_EDGE('',*,*,#3100,.F.);
#4100=ORIENTED_EDGE('',*,*,#3098,.T.);
#4101=ORIENTED_EDGE('',*,*,#3103,.T.);
#4102=ORIENTED_EDGE('',*,*,#3103,.F.);
#4103=ORIENTED_EDGE('',*,*,#3104,.F.);
#4104=ORIENTED_EDGE('',*,*,#3105,.T.);
#4105=ORIENTED_EDGE('',*,*,#3106,.T.);
#4106=ORIENTED_EDGE('',*,*,#3105,.F.);
#4107=ORIENTED_EDGE('',*,*,#3107,.F.);
#4108=ORIENTED_EDGE('',*,*,#3108,.T.);
#4109=ORIENTED_EDGE('',*,*,#3109,.T.);
#4110=ORIENTED_EDGE('',*,*,#3108,.F.);
#4111=ORIENTED_EDGE('',*,*,#3109,.F.);
#4112=ORIENTED_EDGE('',*,*,#3110,.T.);
#4113=ORIENTED_EDGE('',*,*,#3111,.T.);
#4114=ORIENTED_EDGE('',*,*,#3110,.F.);
#4115=ORIENTED_EDGE('',*,*,#3111,.F.);
#4116=ORIENTED_EDGE('',*,*,#3112,.T.);
#4117=ORIENTED_EDGE('',*,*,#3113,.T.);
#4118=ORIENTED_EDGE('',*,*,#3112,.F.);
#4119=ORIENTED_EDGE('',*,*,#3114,.T.);
#4120=ORIENTED_EDGE('',*,*,#3115,.T.);
#4121=ORIENTED_EDGE('',*,*,#3116,.F.);
#4122=ORIENTED_EDGE('',*,*,#3115,.F.);
#4123=ORIENTED_EDGE('',*,*,#3117,.T.);
#4124=ORIENTED_EDGE('',*,*,#3114,.F.);
#4125=ORIENTED_EDGE('',*,*,#3118,.T.);
#4126=ORIENTED_EDGE('',*,*,#3104,.T.);
#4127=ORIENTED_EDGE('',*,*,#3118,.F.);
#4128=ORIENTED_EDGE('',*,*,#3117,.F.);
#4129=ORIENTED_EDGE('',*,*,#3116,.T.);
#4130=ORIENTED_EDGE('',*,*,#3113,.F.);
#4131=ORIENTED_EDGE('',*,*,#3106,.F.);
#4132=ORIENTED_EDGE('',*,*,#3107,.T.);
#4133=ORIENTED_EDGE('',*,*,#3119,.T.);
#4134=ORIENTED_EDGE('',*,*,#3119,.F.);
#4135=ORIENTED_EDGE('',*,*,#3120,.T.);
#4136=ORIENTED_EDGE('',*,*,#3120,.F.);
#4137=ORIENTED_EDGE('',*,*,#3121,.T.);
#4138=ORIENTED_EDGE('',*,*,#3121,.F.);
#4139=ORIENTED_EDGE('',*,*,#3122,.T.);
#4140=ORIENTED_EDGE('',*,*,#3122,.F.);
#4141=ORIENTED_EDGE('',*,*,#3123,.T.);
#4142=ORIENTED_EDGE('',*,*,#3123,.F.);
#4143=ORIENTED_EDGE('',*,*,#3124,.T.);
#4144=ORIENTED_EDGE('',*,*,#3124,.F.);
#4145=ORIENTED_EDGE('',*,*,#3125,.T.);
#4146=ORIENTED_EDGE('',*,*,#3125,.F.);
#4147=ORIENTED_EDGE('',*,*,#3126,.F.);
#4148=ORIENTED_EDGE('',*,*,#3127,.T.);
#4149=ORIENTED_EDGE('',*,*,#3128,.T.);
#4150=ORIENTED_EDGE('',*,*,#3127,.F.);
#4151=ORIENTED_EDGE('',*,*,#3129,.T.);
#4152=ORIENTED_EDGE('',*,*,#3129,.F.);
#4153=ORIENTED_EDGE('',*,*,#3130,.F.);
#4154=ORIENTED_EDGE('',*,*,#3131,.T.);
#4155=ORIENTED_EDGE('',*,*,#3126,.T.);
#4156=ORIENTED_EDGE('',*,*,#3131,.F.);
#4157=ORIENTED_EDGE('',*,*,#3128,.F.);
#4158=ORIENTED_EDGE('',*,*,#3130,.T.);
#4159=ORIENTED_EDGE('',*,*,#3132,.F.);
#4160=ORIENTED_EDGE('',*,*,#3133,.T.);
#4161=ORIENTED_EDGE('',*,*,#3134,.T.);
#4162=ORIENTED_EDGE('',*,*,#3133,.F.);
#4163=ORIENTED_EDGE('',*,*,#3135,.T.);
#4164=ORIENTED_EDGE('',*,*,#3135,.F.);
#4165=ORIENTED_EDGE('',*,*,#3136,.F.);
#4166=ORIENTED_EDGE('',*,*,#3137,.T.);
#4167=ORIENTED_EDGE('',*,*,#3132,.T.);
#4168=ORIENTED_EDGE('',*,*,#3137,.F.);
#4169=ORIENTED_EDGE('',*,*,#3134,.F.);
#4170=ORIENTED_EDGE('',*,*,#3136,.T.);
#4171=ORIENTED_EDGE('',*,*,#3138,.F.);
#4172=ORIENTED_EDGE('',*,*,#3139,.T.);
#4173=ORIENTED_EDGE('',*,*,#3140,.T.);
#4174=ORIENTED_EDGE('',*,*,#3139,.F.);
#4175=ORIENTED_EDGE('',*,*,#3141,.T.);
#4176=ORIENTED_EDGE('',*,*,#3141,.F.);
#4177=ORIENTED_EDGE('',*,*,#3142,.F.);
#4178=ORIENTED_EDGE('',*,*,#3143,.T.);
#4179=ORIENTED_EDGE('',*,*,#3138,.T.);
#4180=ORIENTED_EDGE('',*,*,#3143,.F.);
#4181=ORIENTED_EDGE('',*,*,#3140,.F.);
#4182=ORIENTED_EDGE('',*,*,#3142,.T.);
#4183=ORIENTED_EDGE('',*,*,#3144,.F.);
#4184=ORIENTED_EDGE('',*,*,#3145,.T.);
#4185=ORIENTED_EDGE('',*,*,#3146,.T.);
#4186=ORIENTED_EDGE('',*,*,#3145,.F.);
#4187=ORIENTED_EDGE('',*,*,#3147,.T.);
#4188=ORIENTED_EDGE('',*,*,#3147,.F.);
#4189=ORIENTED_EDGE('',*,*,#3148,.F.);
#4190=ORIENTED_EDGE('',*,*,#3149,.T.);
#4191=ORIENTED_EDGE('',*,*,#3144,.T.);
#4192=ORIENTED_EDGE('',*,*,#3149,.F.);
#4193=ORIENTED_EDGE('',*,*,#3146,.F.);
#4194=ORIENTED_EDGE('',*,*,#3148,.T.);
#4195=ORIENTED_EDGE('',*,*,#3150,.F.);
#4196=ORIENTED_EDGE('',*,*,#3151,.T.);
#4197=ORIENTED_EDGE('',*,*,#3152,.T.);
#4198=ORIENTED_EDGE('',*,*,#3151,.F.);
#4199=ORIENTED_EDGE('',*,*,#3153,.T.);
#4200=ORIENTED_EDGE('',*,*,#3153,.F.);
#4201=ORIENTED_EDGE('',*,*,#3154,.F.);
#4202=ORIENTED_EDGE('',*,*,#3155,.T.);
#4203=ORIENTED_EDGE('',*,*,#3150,.T.);
#4204=ORIENTED_EDGE('',*,*,#3155,.F.);
#4205=ORIENTED_EDGE('',*,*,#3152,.F.);
#4206=ORIENTED_EDGE('',*,*,#3154,.T.);
#4207=ORIENTED_EDGE('',*,*,#3156,.F.);
#4208=ORIENTED_EDGE('',*,*,#3157,.T.);
#4209=ORIENTED_EDGE('',*,*,#3158,.T.);
#4210=ORIENTED_EDGE('',*,*,#3157,.F.);
#4211=ORIENTED_EDGE('',*,*,#3159,.T.);
#4212=ORIENTED_EDGE('',*,*,#3159,.F.);
#4213=ORIENTED_EDGE('',*,*,#3160,.F.);
#4214=ORIENTED_EDGE('',*,*,#3161,.T.);
#4215=ORIENTED_EDGE('',*,*,#3156,.T.);
#4216=ORIENTED_EDGE('',*,*,#3161,.F.);
#4217=ORIENTED_EDGE('',*,*,#3158,.F.);
#4218=ORIENTED_EDGE('',*,*,#3160,.T.);
#4219=ORIENTED_EDGE('',*,*,#3162,.F.);
#4220=ORIENTED_EDGE('',*,*,#3163,.T.);
#4221=ORIENTED_EDGE('',*,*,#3164,.T.);
#4222=ORIENTED_EDGE('',*,*,#3163,.F.);
#4223=ORIENTED_EDGE('',*,*,#3165,.T.);
#4224=ORIENTED_EDGE('',*,*,#3165,.F.);
#4225=ORIENTED_EDGE('',*,*,#3166,.F.);
#4226=ORIENTED_EDGE('',*,*,#3167,.T.);
#4227=ORIENTED_EDGE('',*,*,#3162,.T.);
#4228=ORIENTED_EDGE('',*,*,#3167,.F.);
#4229=ORIENTED_EDGE('',*,*,#3164,.F.);
#4230=ORIENTED_EDGE('',*,*,#3166,.T.);
#4231=ORIENTED_EDGE('',*,*,#3168,.F.);
#4232=ORIENTED_EDGE('',*,*,#3169,.T.);
#4233=ORIENTED_EDGE('',*,*,#3170,.T.);
#4234=ORIENTED_EDGE('',*,*,#3169,.F.);
#4235=ORIENTED_EDGE('',*,*,#3171,.T.);
#4236=ORIENTED_EDGE('',*,*,#3171,.F.);
#4237=ORIENTED_EDGE('',*,*,#3172,.F.);
#4238=ORIENTED_EDGE('',*,*,#3173,.T.);
#4239=ORIENTED_EDGE('',*,*,#3168,.T.);
#4240=ORIENTED_EDGE('',*,*,#3173,.F.);
#4241=ORIENTED_EDGE('',*,*,#3170,.F.);
#4242=ORIENTED_EDGE('',*,*,#3172,.T.);
#4243=ORIENTED_EDGE('',*,*,#3174,.T.);
#4244=ORIENTED_EDGE('',*,*,#3175,.T.);
#4245=ORIENTED_EDGE('',*,*,#3176,.F.);
#4246=ORIENTED_EDGE('',*,*,#3175,.F.);
#4247=ORIENTED_EDGE('',*,*,#3177,.T.);
#4248=ORIENTED_EDGE('',*,*,#3178,.T.);
#4249=ORIENTED_EDGE('',*,*,#3179,.F.);
#4250=ORIENTED_EDGE('',*,*,#3178,.F.);
#4251=ORIENTED_EDGE('',*,*,#3179,.T.);
#4252=ORIENTED_EDGE('',*,*,#3174,.F.);
#4253=ORIENTED_EDGE('',*,*,#3177,.F.);
#4254=ORIENTED_EDGE('',*,*,#3176,.T.);
#4255=ORIENTED_EDGE('',*,*,#3180,.F.);
#4256=ORIENTED_EDGE('',*,*,#3181,.T.);
#4257=ORIENTED_EDGE('',*,*,#3182,.F.);
#4258=ORIENTED_EDGE('',*,*,#3183,.F.);
#4259=ORIENTED_EDGE('',*,*,#3181,.F.);
#4260=ORIENTED_EDGE('',*,*,#3184,.F.);
#4261=ORIENTED_EDGE('',*,*,#3185,.F.);
#4262=ORIENTED_EDGE('',*,*,#3186,.T.);
#4263=ORIENTED_EDGE('',*,*,#3187,.F.);
#4264=ORIENTED_EDGE('',*,*,#3186,.F.);
#4265=ORIENTED_EDGE('',*,*,#3184,.T.);
#4266=ORIENTED_EDGE('',*,*,#3185,.T.);
#4267=ORIENTED_EDGE('',*,*,#3188,.T.);
#4268=ORIENTED_EDGE('',*,*,#3189,.T.);
#4269=ORIENTED_EDGE('',*,*,#3190,.T.);
#4270=ORIENTED_EDGE('',*,*,#3188,.F.);
#4271=ORIENTED_EDGE('',*,*,#3191,.T.);
#4272=ORIENTED_EDGE('',*,*,#3192,.T.);
#4273=ORIENTED_EDGE('',*,*,#3189,.F.);
#4274=ORIENTED_EDGE('',*,*,#3190,.F.);
#4275=ORIENTED_EDGE('',*,*,#3192,.F.);
#4276=ORIENTED_EDGE('',*,*,#3193,.F.);
#4277=ORIENTED_EDGE('',*,*,#3194,.T.);
#4278=ORIENTED_EDGE('',*,*,#3195,.T.);
#4279=ORIENTED_EDGE('',*,*,#3194,.F.);
#4280=ORIENTED_EDGE('',*,*,#3195,.F.);
#4281=ORIENTED_EDGE('',*,*,#3196,.T.);
#4282=ORIENTED_EDGE('',*,*,#3182,.T.);
#4283=ORIENTED_EDGE('',*,*,#3183,.T.);
#4284=ORIENTED_EDGE('',*,*,#3196,.F.);
#4285=ORIENTED_EDGE('',*,*,#3187,.T.);
#4286=ORIENTED_EDGE('',*,*,#3180,.T.);
#4287=ORIENTED_EDGE('',*,*,#3191,.F.);
#4288=ORIENTED_EDGE('',*,*,#3193,.T.);
#4289=ORIENTED_EDGE('',*,*,#3197,.F.);
#4290=ORIENTED_EDGE('',*,*,#3198,.T.);
#4291=ORIENTED_EDGE('',*,*,#3199,.F.);
#4292=ORIENTED_EDGE('',*,*,#3198,.F.);
#4293=ORIENTED_EDGE('',*,*,#3200,.F.);
#4294=ORIENTED_EDGE('',*,*,#3201,.T.);
#4295=ORIENTED_EDGE('',*,*,#3202,.F.);
#4296=ORIENTED_EDGE('',*,*,#3201,.F.);
#4297=ORIENTED_EDGE('',*,*,#3202,.T.);
#4298=ORIENTED_EDGE('',*,*,#3203,.T.);
#4299=ORIENTED_EDGE('',*,*,#3204,.T.);
#4300=ORIENTED_EDGE('',*,*,#3205,.T.);
#4301=ORIENTED_EDGE('',*,*,#3203,.F.);
#4302=ORIENTED_EDGE('',*,*,#3206,.T.);
#4303=ORIENTED_EDGE('',*,*,#3207,.T.);
#4304=ORIENTED_EDGE('',*,*,#3204,.F.);
#4305=ORIENTED_EDGE('',*,*,#3205,.F.);
#4306=ORIENTED_EDGE('',*,*,#3207,.F.);
#4307=ORIENTED_EDGE('',*,*,#3208,.F.);
#4308=ORIENTED_EDGE('',*,*,#3209,.T.);
#4309=ORIENTED_EDGE('',*,*,#3210,.T.);
#4310=ORIENTED_EDGE('',*,*,#3209,.F.);
#4311=ORIENTED_EDGE('',*,*,#3210,.F.);
#4312=ORIENTED_EDGE('',*,*,#3211,.T.);
#4313=ORIENTED_EDGE('',*,*,#3197,.T.);
#4314=ORIENTED_EDGE('',*,*,#3211,.F.);
#4315=ORIENTED_EDGE('',*,*,#3208,.T.);
#4316=ORIENTED_EDGE('',*,*,#3206,.F.);
#4317=ORIENTED_EDGE('',*,*,#3199,.T.);
#4318=ORIENTED_EDGE('',*,*,#3200,.T.);
#4319=ORIENTED_EDGE('',*,*,#3212,.F.);
#4320=ORIENTED_EDGE('',*,*,#3213,.T.);
#4321=ORIENTED_EDGE('',*,*,#3214,.F.);
#4322=ORIENTED_EDGE('',*,*,#3215,.F.);
#4323=ORIENTED_EDGE('',*,*,#3213,.F.);
#4324=ORIENTED_EDGE('',*,*,#3216,.F.);
#4325=ORIENTED_EDGE('',*,*,#3217,.F.);
#4326=ORIENTED_EDGE('',*,*,#3218,.T.);
#4327=ORIENTED_EDGE('',*,*,#3219,.F.);
#4328=ORIENTED_EDGE('',*,*,#3218,.F.);
#4329=ORIENTED_EDGE('',*,*,#3220,.F.);
#4330=ORIENTED_EDGE('',*,*,#3221,.T.);
#4331=ORIENTED_EDGE('',*,*,#3222,.F.);
#4332=ORIENTED_EDGE('',*,*,#3223,.F.);
#4333=ORIENTED_EDGE('',*,*,#3221,.F.);
#4334=ORIENTED_EDGE('',*,*,#3224,.F.);
#4335=ORIENTED_EDGE('',*,*,#3225,.F.);
#4336=ORIENTED_EDGE('',*,*,#3226,.T.);
#4337=ORIENTED_EDGE('',*,*,#3227,.F.);
#4338=ORIENTED_EDGE('',*,*,#3226,.F.);
#4339=ORIENTED_EDGE('',*,*,#3228,.F.);
#4340=ORIENTED_EDGE('',*,*,#3229,.T.);
#4341=ORIENTED_EDGE('',*,*,#3230,.F.);
#4342=ORIENTED_EDGE('',*,*,#3231,.F.);
#4343=ORIENTED_EDGE('',*,*,#3229,.F.);
#4344=ORIENTED_EDGE('',*,*,#3232,.F.);
#4345=ORIENTED_EDGE('',*,*,#3233,.F.);
#4346=ORIENTED_EDGE('',*,*,#3234,.T.);
#4347=ORIENTED_EDGE('',*,*,#3235,.F.);
#4348=ORIENTED_EDGE('',*,*,#3234,.F.);
#4349=ORIENTED_EDGE('',*,*,#3236,.F.);
#4350=ORIENTED_EDGE('',*,*,#3237,.T.);
#4351=ORIENTED_EDGE('',*,*,#3238,.F.);
#4352=ORIENTED_EDGE('',*,*,#3239,.F.);
#4353=ORIENTED_EDGE('',*,*,#3237,.F.);
#4354=ORIENTED_EDGE('',*,*,#3240,.F.);
#4355=ORIENTED_EDGE('',*,*,#3241,.F.);
#4356=ORIENTED_EDGE('',*,*,#3242,.T.);
#4357=ORIENTED_EDGE('',*,*,#3243,.F.);
#4358=ORIENTED_EDGE('',*,*,#3242,.F.);
#4359=ORIENTED_EDGE('',*,*,#3244,.F.);
#4360=ORIENTED_EDGE('',*,*,#3245,.T.);
#4361=ORIENTED_EDGE('',*,*,#3246,.F.);
#4362=ORIENTED_EDGE('',*,*,#3247,.F.);
#4363=ORIENTED_EDGE('',*,*,#3248,.F.);
#4364=ORIENTED_EDGE('',*,*,#3249,.T.);
#4365=ORIENTED_EDGE('',*,*,#3250,.F.);
#4366=ORIENTED_EDGE('',*,*,#3245,.F.);
#4367=ORIENTED_EDGE('',*,*,#3251,.F.);
#4368=ORIENTED_EDGE('',*,*,#3252,.F.);
#4369=ORIENTED_EDGE('',*,*,#3253,.F.);
#4370=ORIENTED_EDGE('',*,*,#3249,.F.);
#4371=ORIENTED_EDGE('',*,*,#3247,.T.);
#4372=ORIENTED_EDGE('',*,*,#3254,.T.);
#4373=ORIENTED_EDGE('',*,*,#3255,.F.);
#4374=ORIENTED_EDGE('',*,*,#3256,.T.);
#4375=ORIENTED_EDGE('',*,*,#3219,.T.);
#4376=ORIENTED_EDGE('',*,*,#3235,.T.);
#4377=ORIENTED_EDGE('',*,*,#3252,.T.);
#4378=ORIENTED_EDGE('',*,*,#3257,.T.);
#4379=ORIENTED_EDGE('',*,*,#3258,.T.);
#4380=ORIENTED_EDGE('',*,*,#3259,.T.);
#4381=ORIENTED_EDGE('',*,*,#3251,.T.);
#4382=ORIENTED_EDGE('',*,*,#3248,.T.);
#4383=ORIENTED_EDGE('',*,*,#3244,.T.);
#4384=ORIENTED_EDGE('',*,*,#3256,.F.);
#4385=ORIENTED_EDGE('',*,*,#3260,.F.);
#4386=ORIENTED_EDGE('',*,*,#3261,.T.);
#4387=ORIENTED_EDGE('',*,*,#3262,.F.);
#4388=ORIENTED_EDGE('',*,*,#3263,.F.);
#4389=ORIENTED_EDGE('',*,*,#3264,.T.);
#4390=ORIENTED_EDGE('',*,*,#3265,.T.);
#4391=ORIENTED_EDGE('',*,*,#3266,.T.);
#4392=ORIENTED_EDGE('',*,*,#3267,.F.);
#4393=ORIENTED_EDGE('',*,*,#3268,.T.);
#4394=ORIENTED_EDGE('',*,*,#3269,.T.);
#4395=ORIENTED_EDGE('',*,*,#3270,.T.);
#4396=ORIENTED_EDGE('',*,*,#3271,.F.);
#4397=ORIENTED_EDGE('',*,*,#3272,.F.);
#4398=ORIENTED_EDGE('',*,*,#3273,.F.);
#4399=ORIENTED_EDGE('',*,*,#3274,.F.);
#4400=ORIENTED_EDGE('',*,*,#3275,.F.);
#4401=ORIENTED_EDGE('',*,*,#3276,.T.);
#4402=ORIENTED_EDGE('',*,*,#3277,.T.);
#4403=ORIENTED_EDGE('',*,*,#3278,.T.);
#4404=ORIENTED_EDGE('',*,*,#3257,.F.);
#4405=ORIENTED_EDGE('',*,*,#3279,.T.);
#4406=ORIENTED_EDGE('',*,*,#3280,.T.);
#4407=ORIENTED_EDGE('',*,*,#3281,.T.);
#4408=ORIENTED_EDGE('',*,*,#3276,.F.);
#4409=ORIENTED_EDGE('',*,*,#3282,.F.);
#4410=ORIENTED_EDGE('',*,*,#3283,.F.);
#4411=ORIENTED_EDGE('',*,*,#3284,.F.);
#4412=ORIENTED_EDGE('',*,*,#3277,.F.);
#4413=ORIENTED_EDGE('',*,*,#3284,.T.);
#4414=ORIENTED_EDGE('',*,*,#3285,.F.);
#4415=ORIENTED_EDGE('',*,*,#3286,.F.);
#4416=ORIENTED_EDGE('',*,*,#3278,.F.);
#4417=ORIENTED_EDGE('',*,*,#3286,.T.);
#4418=ORIENTED_EDGE('',*,*,#3287,.F.);
#4419=ORIENTED_EDGE('',*,*,#3258,.F.);
#4420=ORIENTED_EDGE('',*,*,#3253,.T.);
#4421=ORIENTED_EDGE('',*,*,#3259,.F.);
#4422=ORIENTED_EDGE('',*,*,#3287,.T.);
#4423=ORIENTED_EDGE('',*,*,#3285,.T.);
#4424=ORIENTED_EDGE('',*,*,#3283,.T.);
#4425=ORIENTED_EDGE('',*,*,#3288,.F.);
#4426=ORIENTED_EDGE('',*,*,#3289,.F.);
#4427=ORIENTED_EDGE('',*,*,#3290,.F.);
#4428=ORIENTED_EDGE('',*,*,#3291,.F.);
#4429=ORIENTED_EDGE('',*,*,#3292,.F.);
#4430=ORIENTED_EDGE('',*,*,#3293,.T.);
#4431=ORIENTED_EDGE('',*,*,#3294,.T.);
#4432=ORIENTED_EDGE('',*,*,#3295,.T.);
#4433=ORIENTED_EDGE('',*,*,#3296,.F.);
#4434=ORIENTED_EDGE('',*,*,#3297,.T.);
#4435=ORIENTED_EDGE('',*,*,#3298,.T.);
#4436=ORIENTED_EDGE('',*,*,#3299,.T.);
#4437=ORIENTED_EDGE('',*,*,#3300,.F.);
#4438=ORIENTED_EDGE('',*,*,#3301,.F.);
#4439=ORIENTED_EDGE('',*,*,#3302,.F.);
#4440=ORIENTED_EDGE('',*,*,#3303,.F.);
#4441=ORIENTED_EDGE('',*,*,#3254,.F.);
#4442=ORIENTED_EDGE('',*,*,#3246,.T.);
#4443=ORIENTED_EDGE('',*,*,#3250,.T.);
#4444=ORIENTED_EDGE('',*,*,#3304,.T.);
#4445=ORIENTED_EDGE('',*,*,#3305,.T.);
#4446=ORIENTED_EDGE('',*,*,#3306,.T.);
#4447=ORIENTED_EDGE('',*,*,#3282,.T.);
#4448=ORIENTED_EDGE('',*,*,#3275,.T.);
#4449=ORIENTED_EDGE('',*,*,#3307,.F.);
#4450=ORIENTED_EDGE('',*,*,#3288,.T.);
#4451=ORIENTED_EDGE('',*,*,#3227,.T.);
#4452=ORIENTED_EDGE('',*,*,#3243,.T.);
#4453=ORIENTED_EDGE('',*,*,#3264,.F.);
#4454=ORIENTED_EDGE('',*,*,#3308,.F.);
#4455=ORIENTED_EDGE('',*,*,#3299,.F.);
#4456=ORIENTED_EDGE('',*,*,#3309,.F.);
#4457=ORIENTED_EDGE('',*,*,#3265,.F.);
#4458=ORIENTED_EDGE('',*,*,#3309,.T.);
#4459=ORIENTED_EDGE('',*,*,#3298,.F.);
#4460=ORIENTED_EDGE('',*,*,#3310,.F.);
#4461=ORIENTED_EDGE('',*,*,#3266,.F.);
#4462=ORIENTED_EDGE('',*,*,#3310,.T.);
#4463=ORIENTED_EDGE('',*,*,#3297,.F.);
#4464=ORIENTED_EDGE('',*,*,#3311,.F.);
#4465=ORIENTED_EDGE('',*,*,#3308,.T.);
#4466=ORIENTED_EDGE('',*,*,#3263,.T.);
#4467=ORIENTED_EDGE('',*,*,#3312,.F.);
#4468=ORIENTED_EDGE('',*,*,#3300,.T.);
#4469=ORIENTED_EDGE('',*,*,#3212,.T.);
#4470=ORIENTED_EDGE('',*,*,#3228,.T.);
#4471=ORIENTED_EDGE('',*,*,#3311,.T.);
#4472=ORIENTED_EDGE('',*,*,#3296,.T.);
#4473=ORIENTED_EDGE('',*,*,#3313,.T.);
#4474=ORIENTED_EDGE('',*,*,#3267,.T.);
#4475=ORIENTED_EDGE('',*,*,#3270,.F.);
#4476=ORIENTED_EDGE('',*,*,#3314,.T.);
#4477=ORIENTED_EDGE('',*,*,#3293,.F.);
#4478=ORIENTED_EDGE('',*,*,#3315,.F.);
#4479=ORIENTED_EDGE('',*,*,#3269,.F.);
#4480=ORIENTED_EDGE('',*,*,#3316,.T.);
#4481=ORIENTED_EDGE('',*,*,#3294,.F.);
#4482=ORIENTED_EDGE('',*,*,#3314,.F.);
#4483=ORIENTED_EDGE('',*,*,#3268,.F.);
#4484=ORIENTED_EDGE('',*,*,#3313,.F.);
#4485=ORIENTED_EDGE('',*,*,#3295,.F.);
#4486=ORIENTED_EDGE('',*,*,#3316,.F.);
#4487=ORIENTED_EDGE('',*,*,#3315,.T.);
#4488=ORIENTED_EDGE('',*,*,#3292,.T.);
#4489=ORIENTED_EDGE('',*,*,#3317,.F.);
#4490=ORIENTED_EDGE('',*,*,#3271,.T.);
#4491=ORIENTED_EDGE('',*,*,#3220,.T.);
#4492=ORIENTED_EDGE('',*,*,#3236,.T.);
#4493=ORIENTED_EDGE('',*,*,#3279,.F.);
#4494=ORIENTED_EDGE('',*,*,#3318,.T.);
#4495=ORIENTED_EDGE('',*,*,#3304,.F.);
#4496=ORIENTED_EDGE('',*,*,#3318,.F.);
#4497=ORIENTED_EDGE('',*,*,#3224,.T.);
#4498=ORIENTED_EDGE('',*,*,#3225,.T.);
#4499=ORIENTED_EDGE('',*,*,#3222,.T.);
#4500=ORIENTED_EDGE('',*,*,#3223,.T.);
#4501=ORIENTED_EDGE('',*,*,#3240,.T.);
#4502=ORIENTED_EDGE('',*,*,#3241,.T.);
#4503=ORIENTED_EDGE('',*,*,#3238,.T.);
#4504=ORIENTED_EDGE('',*,*,#3239,.T.);
#4505=ORIENTED_EDGE('',*,*,#3305,.F.);
#4506=ORIENTED_EDGE('',*,*,#3319,.T.);
#4507=ORIENTED_EDGE('',*,*,#3280,.F.);
#4508=ORIENTED_EDGE('',*,*,#3319,.F.);
#4509=ORIENTED_EDGE('',*,*,#3216,.T.);
#4510=ORIENTED_EDGE('',*,*,#3217,.T.);
#4511=ORIENTED_EDGE('',*,*,#3214,.T.);
#4512=ORIENTED_EDGE('',*,*,#3215,.T.);
#4513=ORIENTED_EDGE('',*,*,#3232,.T.);
#4514=ORIENTED_EDGE('',*,*,#3233,.T.);
#4515=ORIENTED_EDGE('',*,*,#3230,.T.);
#4516=ORIENTED_EDGE('',*,*,#3231,.T.);
#4517=ORIENTED_EDGE('',*,*,#3306,.F.);
#4518=ORIENTED_EDGE('',*,*,#3320,.T.);
#4519=ORIENTED_EDGE('',*,*,#3281,.F.);
#4520=ORIENTED_EDGE('',*,*,#3320,.F.);
#4521=ORIENTED_EDGE('',*,*,#3289,.T.);
#4522=ORIENTED_EDGE('',*,*,#3307,.T.);
#4523=ORIENTED_EDGE('',*,*,#3274,.T.);
#4524=ORIENTED_EDGE('',*,*,#3321,.T.);
#4525=ORIENTED_EDGE('',*,*,#3321,.F.);
#4526=ORIENTED_EDGE('',*,*,#3273,.T.);
#4527=ORIENTED_EDGE('',*,*,#3322,.F.);
#4528=ORIENTED_EDGE('',*,*,#3290,.T.);
#4529=ORIENTED_EDGE('',*,*,#3272,.T.);
#4530=ORIENTED_EDGE('',*,*,#3317,.T.);
#4531=ORIENTED_EDGE('',*,*,#3291,.T.);
#4532=ORIENTED_EDGE('',*,*,#3322,.T.);
#4533=ORIENTED_EDGE('',*,*,#3260,.T.);
#4534=ORIENTED_EDGE('',*,*,#3255,.T.);
#4535=ORIENTED_EDGE('',*,*,#3303,.T.);
#4536=ORIENTED_EDGE('',*,*,#3323,.T.);
#4537=ORIENTED_EDGE('',*,*,#3323,.F.);
#4538=ORIENTED_EDGE('',*,*,#3302,.T.);
#4539=ORIENTED_EDGE('',*,*,#3324,.F.);
#4540=ORIENTED_EDGE('',*,*,#3261,.F.);
#4541=ORIENTED_EDGE('',*,*,#3301,.T.);
#4542=ORIENTED_EDGE('',*,*,#3312,.T.);
#4543=ORIENTED_EDGE('',*,*,#3262,.T.);
#4544=ORIENTED_EDGE('',*,*,#3324,.T.);
#4545=CYLINDRICAL_SURFACE('',#5124,6.00000000000001);
#4546=CYLINDRICAL_SURFACE('',#5129,4.);
#4547=CYLINDRICAL_SURFACE('',#5133,4.);
#4548=CYLINDRICAL_SURFACE('',#5137,5.);
#4549=CYLINDRICAL_SURFACE('',#5142,3.00000000000001);
#4550=CYLINDRICAL_SURFACE('',#5144,3.00000000000001);
#4551=CYLINDRICAL_SURFACE('',#5148,4.99999999999977);
#4552=CYLINDRICAL_SURFACE('',#5150,4.99999999999977);
#4553=CYLINDRICAL_SURFACE('',#5162,1.);
#4554=CYLINDRICAL_SURFACE('',#5165,1.);
#4555=CYLINDRICAL_SURFACE('',#5167,1.);
#4556=CYLINDRICAL_SURFACE('',#5176,1.);
#4557=CYLINDRICAL_SURFACE('',#5184,1.);
#4558=CYLINDRICAL_SURFACE('',#5190,1.);
#4559=CYLINDRICAL_SURFACE('',#5191,1.);
#4560=CYLINDRICAL_SURFACE('',#5195,1.);
#4561=CYLINDRICAL_SURFACE('',#5197,1.);
#4562=CYLINDRICAL_SURFACE('',#5198,1.);
#4563=CYLINDRICAL_SURFACE('',#5199,1.);
#4564=CYLINDRICAL_SURFACE('',#5200,1.);
#4565=CYLINDRICAL_SURFACE('',#5201,1.);
#4566=CYLINDRICAL_SURFACE('',#5208,6.00000000000001);
#4567=CYLINDRICAL_SURFACE('',#5211,7.50000000000001);
#4568=CYLINDRICAL_SURFACE('',#5214,6.00000000000001);
#4569=CYLINDRICAL_SURFACE('',#5219,4.);
#4570=CYLINDRICAL_SURFACE('',#5223,4.);
#4571=CYLINDRICAL_SURFACE('',#5227,4.99999999999977);
#4572=CYLINDRICAL_SURFACE('',#5232,4.99999999999977);
#4573=CYLINDRICAL_SURFACE('',#5237,3.);
#4574=CYLINDRICAL_SURFACE('',#5238,3.);
#4575=CYLINDRICAL_SURFACE('',#5256,1.);
#4576=CYLINDRICAL_SURFACE('',#5265,1.);
#4577=CYLINDRICAL_SURFACE('',#5270,1.);
#4578=CYLINDRICAL_SURFACE('',#5271,1.);
#4579=CYLINDRICAL_SURFACE('',#5276,1.);
#4580=CYLINDRICAL_SURFACE('',#5277,1.);
#4581=CYLINDRICAL_SURFACE('',#5278,1.);
#4582=CYLINDRICAL_SURFACE('',#5279,1.);
#4583=CYLINDRICAL_SURFACE('',#5280,1.);
#4584=CYLINDRICAL_SURFACE('',#5281,1.);
#4585=CYLINDRICAL_SURFACE('',#5282,1.);
#4586=CYLINDRICAL_SURFACE('',#5283,1.);
#4587=CYLINDRICAL_SURFACE('',#5292,6.00000000000001);
#4588=CYLINDRICAL_SURFACE('',#5295,7.50000000000001);
#4589=CYLINDRICAL_SURFACE('',#5306,6.);
#4590=CYLINDRICAL_SURFACE('',#5311,7.24999999999999);
#4591=CYLINDRICAL_SURFACE('',#5313,7.24999999999999);
#4592=CYLINDRICAL_SURFACE('',#5322,9.25000000000001);
#4593=CYLINDRICAL_SURFACE('',#5328,9.25);
#4594=CYLINDRICAL_SURFACE('',#5334,10.5);
#4595=CYLINDRICAL_SURFACE('',#5445,8.25);
#4596=CYLINDRICAL_SURFACE('',#5448,8.75);
#4597=CYLINDRICAL_SURFACE('',#5485,9.1);
#4598=CYLINDRICAL_SURFACE('',#5493,7.39999999999999);
#4599=CYLINDRICAL_SURFACE('',#5504,7.39999999999999);
#4600=CYLINDRICAL_SURFACE('',#5512,9.1);
#4601=CYLINDRICAL_SURFACE('',#5524,4.99999999999977);
#4602=CYLINDRICAL_SURFACE('',#5538,2.942);
#4603=CYLINDRICAL_SURFACE('',#5543,3.);
#4604=CYLINDRICAL_SURFACE('',#5547,3.);
#4605=CYLINDRICAL_SURFACE('',#5553,6.00000000000001);
#4606=CYLINDRICAL_SURFACE('',#5559,7.50000000000001);
#4607=CYLINDRICAL_SURFACE('',#5563,3.);
#4608=CYLINDRICAL_SURFACE('',#5567,3.);
#4609=CYLINDRICAL_SURFACE('',#5573,6.00000000000001);
#4610=CYLINDRICAL_SURFACE('',#5584,7.5);
#4611=CYLINDRICAL_SURFACE('',#5589,11.);
#4612=CYLINDRICAL_SURFACE('',#5591,11.);
#4613=CYLINDRICAL_SURFACE('',#5600,14.);
#4614=CYLINDRICAL_SURFACE('',#5606,14.);
#4615=CYLINDRICAL_SURFACE('',#5612,17.5);
#4616=CYLINDRICAL_SURFACE('',#5709,12.5);
#4617=CYLINDRICAL_SURFACE('',#5712,13.25);
#4618=CYLINDRICAL_SURFACE('',#5727,13.775);
#4619=CYLINDRICAL_SURFACE('',#5735,11.225);
#4620=CYLINDRICAL_SURFACE('',#5746,11.225);
#4621=CYLINDRICAL_SURFACE('',#5754,13.775);
#4622=CYLINDRICAL_SURFACE('',#5758,2.5);
#4623=CYLINDRICAL_SURFACE('',#5760,2.5);
#4624=CYLINDRICAL_SURFACE('',#5762,2.5);
#4625=CYLINDRICAL_SURFACE('',#5764,2.5);
#4626=CYLINDRICAL_SURFACE('',#5766,2.5);
#4627=CYLINDRICAL_SURFACE('',#5768,2.5);
#4628=CYLINDRICAL_SURFACE('',#5770,2.5);
#4629=CYLINDRICAL_SURFACE('',#5772,2.5);
#4630=CYLINDRICAL_SURFACE('',#5800,10.5);
#4631=CYLINDRICAL_SURFACE('',#5801,10.5);
#4632=CYLINDRICAL_SURFACE('',#5802,17.5);
#4633=ADVANCED_FACE('',(#622),#4545,.F.);
#4634=ADVANCED_FACE('',(#623,#333),#482,.T.);
#4635=ADVANCED_FACE('',(#624),#4546,.F.);
#4636=ADVANCED_FACE('',(#625),#483,.T.);
#4637=ADVANCED_FACE('',(#626),#4547,.F.);
#4638=ADVANCED_FACE('',(#627),#484,.T.);
#4639=ADVANCED_FACE('',(#628),#4548,.F.);
#4640=ADVANCED_FACE('',(#629,#334),#485,.T.);
#4641=ADVANCED_FACE('',(#630),#4549,.F.);
#4642=ADVANCED_FACE('',(#631),#4550,.F.);
#4643=ADVANCED_FACE('',(#632),#486,.T.);
#4644=ADVANCED_FACE('',(#633),#4551,.F.);
#4645=ADVANCED_FACE('',(#634),#4552,.F.);
#4646=ADVANCED_FACE('',(#635,#335),#487,.T.);
#4647=ADVANCED_FACE('',(#636,#336),#488,.F.);
#4648=ADVANCED_FACE('',(#637),#489,.T.);
#4649=ADVANCED_FACE('',(#638,#337),#490,.F.);
#4650=ADVANCED_FACE('',(#639),#4553,.T.);
#4651=ADVANCED_FACE('',(#640,#338,#339),#491,.T.);
#4652=ADVANCED_FACE('',(#641),#4554,.T.);
#4653=ADVANCED_FACE('',(#642),#4555,.T.);
#4654=ADVANCED_FACE('',(#643),#279,.T.);
#4655=ADVANCED_FACE('',(#644),#280,.T.);
#4656=ADVANCED_FACE('',(#645),#4556,.T.);
#4657=ADVANCED_FACE('',(#646),#281,.T.);
#4658=ADVANCED_FACE('',(#647),#282,.T.);
#4659=ADVANCED_FACE('',(#648),#4557,.T.);
#4660=ADVANCED_FACE('',(#649),#283,.T.);
#4661=ADVANCED_FACE('',(#650),#4558,.T.);
#4662=ADVANCED_FACE('',(#651),#4559,.T.);
#4663=ADVANCED_FACE('',(#652),#284,.T.);
#4664=ADVANCED_FACE('',(#653),#4560,.T.);
#4665=ADVANCED_FACE('',(#654),#4561,.T.);
#4666=ADVANCED_FACE('',(#655),#4562,.T.);
#4667=ADVANCED_FACE('',(#656),#4563,.T.);
#4668=ADVANCED_FACE('',(#657),#4564,.T.);
#4669=ADVANCED_FACE('',(#658),#4565,.T.);
#4670=ADVANCED_FACE('',(#659),#492,.T.);
#4671=ADVANCED_FACE('',(#660,#340,#341),#493,.T.);
#4672=ADVANCED_FACE('',(#661,#342),#494,.T.);
#4673=ADVANCED_FACE('',(#662),#495,.T.);
#4674=ADVANCED_FACE('',(#663),#4566,.F.);
#4675=ADVANCED_FACE('',(#664),#496,.T.);
#4676=ADVANCED_FACE('',(#665),#4567,.F.);
#4677=ADVANCED_FACE('',(#666),#497,.T.);
#4678=ADVANCED_FACE('',(#667),#4568,.F.);
#4679=ADVANCED_FACE('',(#668,#343),#498,.F.);
#4680=ADVANCED_FACE('',(#669),#4569,.F.);
#4681=ADVANCED_FACE('',(#670),#499,.T.);
#4682=ADVANCED_FACE('',(#671),#4570,.F.);
#4683=ADVANCED_FACE('',(#672),#500,.T.);
#4684=ADVANCED_FACE('',(#673),#4571,.F.);
#4685=ADVANCED_FACE('',(#674,#344),#501,.T.);
#4686=ADVANCED_FACE('',(#675),#4572,.F.);
#4687=ADVANCED_FACE('',(#676,#345),#502,.T.);
#4688=ADVANCED_FACE('',(#677),#4573,.F.);
#4689=ADVANCED_FACE('',(#678),#4574,.F.);
#4690=ADVANCED_FACE('',(#679),#285,.T.);
#4691=ADVANCED_FACE('',(#680),#286,.T.);
#4692=ADVANCED_FACE('',(#681),#287,.T.);
#4693=ADVANCED_FACE('',(#682),#288,.T.);
#4694=ADVANCED_FACE('',(#683),#4575,.T.);
#4695=ADVANCED_FACE('',(#684),#289,.T.);
#4696=ADVANCED_FACE('',(#685),#290,.T.);
#4697=ADVANCED_FACE('',(#686),#4576,.T.);
#4698=ADVANCED_FACE('',(#687),#291,.T.);
#4699=ADVANCED_FACE('',(#688),#4577,.T.);
#4700=ADVANCED_FACE('',(#689),#4578,.T.);
#4701=ADVANCED_FACE('',(#690),#292,.T.);
#4702=ADVANCED_FACE('',(#691),#4579,.T.);
#4703=ADVANCED_FACE('',(#692),#4580,.T.);
#4704=ADVANCED_FACE('',(#693),#4581,.T.);
#4705=ADVANCED_FACE('',(#694),#4582,.T.);
#4706=ADVANCED_FACE('',(#695),#4583,.T.);
#4707=ADVANCED_FACE('',(#696),#4584,.T.);
#4708=ADVANCED_FACE('',(#697),#4585,.T.);
#4709=ADVANCED_FACE('',(#698),#4586,.T.);
#4710=ADVANCED_FACE('',(#699,#346,#347,#348),#503,.T.);
#4711=ADVANCED_FACE('',(#700),#504,.T.);
#4712=ADVANCED_FACE('',(#701,#349,#350),#505,.T.);
#4713=ADVANCED_FACE('',(#702),#506,.T.);
#4714=ADVANCED_FACE('',(#703,#351,#352),#507,.T.);
#4715=ADVANCED_FACE('',(#704),#508,.T.);
#4716=ADVANCED_FACE('',(#705),#4587,.F.);
#4717=ADVANCED_FACE('',(#706,#353),#509,.F.);
#4718=ADVANCED_FACE('',(#707),#4588,.F.);
#4719=ADVANCED_FACE('',(#708),#510,.F.);
#4720=ADVANCED_FACE('',(#709),#124,.F.);
#4721=ADVANCED_FACE('',(#710),#107,.F.);
#4722=ADVANCED_FACE('',(#711),#4589,.F.);
#4723=ADVANCED_FACE('',(#712),#108,.F.);
#4724=ADVANCED_FACE('',(#713),#4590,.T.);
#4725=ADVANCED_FACE('',(#714),#4591,.T.);
#4726=ADVANCED_FACE('',(#715,#354),#511,.T.);
#4727=ADVANCED_FACE('',(#716,#355),#512,.T.);
#4728=ADVANCED_FACE('',(#717),#293,.T.);
#4729=ADVANCED_FACE('',(#718),#109,.T.);
#4730=ADVANCED_FACE('',(#719),#4592,.F.);
#4731=ADVANCED_FACE('',(#720),#125,.F.);
#4732=ADVANCED_FACE('',(#721),#4593,.F.);
#4733=ADVANCED_FACE('',(#722),#110,.T.);
#4734=ADVANCED_FACE('',(#723),#4594,.T.);
#4735=ADVANCED_FACE('',(#724,#356),#513,.T.);
#4736=ADVANCED_FACE('',(#725,#357),#514,.T.);
#4737=ADVANCED_FACE('',(#726),#294,.T.);
#4738=ADVANCED_FACE('',(#727),#295,.T.);
#4739=ADVANCED_FACE('',(#728),#296,.T.);
#4740=ADVANCED_FACE('',(#729),#297,.T.);
#4741=ADVANCED_FACE('',(#730),#298,.T.);
#4742=ADVANCED_FACE('',(#731),#299,.T.);
#4743=ADVANCED_FACE('',(#732),#300,.T.);
#4744=ADVANCED_FACE('',(#733),#301,.T.);
#4745=ADVANCED_FACE('',(#734),#302,.T.);
#4746=ADVANCED_FACE('',(#735),#95,.F.);
#4747=ADVANCED_FACE('',(#736,#358,#359),#303,.F.);
#4748=ADVANCED_FACE('',(#737,#360),#515,.F.);
#4749=ADVANCED_FACE('',(#738,#361),#516,.F.);
#4750=ADVANCED_FACE('',(#739),#96,.F.);
#4751=ADVANCED_FACE('',(#740,#362,#363),#304,.F.);
#4752=ADVANCED_FACE('',(#741,#364),#517,.F.);
#4753=ADVANCED_FACE('',(#742,#365),#518,.F.);
#4754=ADVANCED_FACE('',(#743),#97,.F.);
#4755=ADVANCED_FACE('',(#744,#366,#367),#305,.F.);
#4756=ADVANCED_FACE('',(#745,#368),#519,.F.);
#4757=ADVANCED_FACE('',(#746,#369),#520,.F.);
#4758=ADVANCED_FACE('',(#747),#98,.F.);
#4759=ADVANCED_FACE('',(#748,#370,#371),#306,.F.);
#4760=ADVANCED_FACE('',(#749,#372),#521,.F.);
#4761=ADVANCED_FACE('',(#750,#373),#522,.F.);
#4762=ADVANCED_FACE('',(#751),#99,.F.);
#4763=ADVANCED_FACE('',(#752,#374,#375),#307,.F.);
#4764=ADVANCED_FACE('',(#753,#376),#523,.F.);
#4765=ADVANCED_FACE('',(#754,#377),#524,.F.);
#4766=ADVANCED_FACE('',(#755),#100,.F.);
#4767=ADVANCED_FACE('',(#756,#378,#379),#308,.F.);
#4768=ADVANCED_FACE('',(#757,#380),#525,.F.);
#4769=ADVANCED_FACE('',(#758,#381),#526,.F.);
#4770=ADVANCED_FACE('',(#759),#101,.F.);
#4771=ADVANCED_FACE('',(#760,#382,#383),#309,.F.);
#4772=ADVANCED_FACE('',(#761,#384),#527,.F.);
#4773=ADVANCED_FACE('',(#762,#385),#528,.F.);
#4774=ADVANCED_FACE('',(#763),#102,.F.);
#4775=ADVANCED_FACE('',(#764,#386,#387),#310,.F.);
#4776=ADVANCED_FACE('',(#765,#388),#529,.F.);
#4777=ADVANCED_FACE('',(#766,#389),#530,.F.);
#4778=ADVANCED_FACE('',(#767),#103,.F.);
#4779=ADVANCED_FACE('',(#768,#390,#391),#311,.F.);
#4780=ADVANCED_FACE('',(#769,#392),#531,.F.);
#4781=ADVANCED_FACE('',(#770,#393),#532,.F.);
#4782=ADVANCED_FACE('',(#771),#104,.F.);
#4783=ADVANCED_FACE('',(#772,#394,#395),#312,.F.);
#4784=ADVANCED_FACE('',(#773,#396),#533,.F.);
#4785=ADVANCED_FACE('',(#774,#397),#534,.F.);
#4786=ADVANCED_FACE('',(#775),#4595,.F.);
#4787=ADVANCED_FACE('',(#776),#4596,.T.);
#4788=ADVANCED_FACE('',(#777,#398),#535,.F.);
#4789=ADVANCED_FACE('',(#778,#399),#536,.T.);
#4790=ADVANCED_FACE('',(#779),#105,.F.);
#4791=ADVANCED_FACE('',(#780,#400,#401),#313,.F.);
#4792=ADVANCED_FACE('',(#781,#402),#537,.F.);
#4793=ADVANCED_FACE('',(#782,#403),#538,.F.);
#4794=ADVANCED_FACE('',(#783),#106,.F.);
#4795=ADVANCED_FACE('',(#784,#404,#405),#314,.F.);
#4796=ADVANCED_FACE('',(#785,#406),#539,.F.);
#4797=ADVANCED_FACE('',(#786,#407),#540,.F.);
#4798=ADVANCED_FACE('',(#787),#315,.T.);
#4799=ADVANCED_FACE('',(#788),#316,.T.);
#4800=ADVANCED_FACE('',(#789),#126,.T.);
#4801=ADVANCED_FACE('',(#790),#127,.T.);
#4802=ADVANCED_FACE('',(#791),#4597,.T.);
#4803=ADVANCED_FACE('',(#792),#111,.T.);
#4804=ADVANCED_FACE('',(#793),#112,.F.);
#4805=ADVANCED_FACE('',(#794),#4598,.F.);
#4806=ADVANCED_FACE('',(#795,#408),#541,.T.);
#4807=ADVANCED_FACE('',(#796,#409),#542,.T.);
#4808=ADVANCED_FACE('',(#797),#128,.T.);
#4809=ADVANCED_FACE('',(#798),#129,.T.);
#4810=ADVANCED_FACE('',(#799),#4599,.F.);
#4811=ADVANCED_FACE('',(#800),#113,.F.);
#4812=ADVANCED_FACE('',(#801),#114,.T.);
#4813=ADVANCED_FACE('',(#802),#4600,.T.);
#4814=ADVANCED_FACE('',(#803,#410),#543,.T.);
#4815=ADVANCED_FACE('',(#804,#411),#544,.T.);
#4816=ADVANCED_FACE('',(#805),#115,.T.);
#4817=ADVANCED_FACE('',(#806),#130,.T.);
#4818=ADVANCED_FACE('',(#807,#412),#545,.T.);
#4819=ADVANCED_FACE('',(#808),#4601,.T.);
#4820=ADVANCED_FACE('',(#809),#546,.F.);
#4821=ADVANCED_FACE('',(#810),#547,.F.);
#4822=ADVANCED_FACE('',(#811),#548,.F.);
#4823=ADVANCED_FACE('',(#812),#549,.F.);
#4824=ADVANCED_FACE('',(#813),#550,.F.);
#4825=ADVANCED_FACE('',(#814),#551,.F.);
#4826=ADVANCED_FACE('',(#815),#552,.F.);
#4827=ADVANCED_FACE('',(#816),#553,.F.);
#4828=ADVANCED_FACE('',(#817),#554,.F.);
#4829=ADVANCED_FACE('',(#818),#555,.F.);
#4830=ADVANCED_FACE('',(#819),#556,.F.);
#4831=ADVANCED_FACE('',(#820),#557,.F.);
#4832=ADVANCED_FACE('',(#821),#4602,.T.);
#4833=ADVANCED_FACE('',(#822),#558,.T.);
#4834=ADVANCED_FACE('',(#823,#413),#559,.T.);
#4835=ADVANCED_FACE('',(#824),#4603,.F.);
#4836=ADVANCED_FACE('',(#825),#560,.T.);
#4837=ADVANCED_FACE('',(#826),#4604,.F.);
#4838=ADVANCED_FACE('',(#827),#561,.T.);
#4839=ADVANCED_FACE('',(#828,#414),#562,.T.);
#4840=ADVANCED_FACE('',(#829),#4605,.T.);
#4841=ADVANCED_FACE('',(#830,#415),#563,.F.);
#4842=ADVANCED_FACE('',(#831),#564,.F.);
#4843=ADVANCED_FACE('',(#832),#4606,.T.);
#4844=ADVANCED_FACE('',(#833),#565,.T.);
#4845=ADVANCED_FACE('',(#834),#4607,.F.);
#4846=ADVANCED_FACE('',(#835),#566,.T.);
#4847=ADVANCED_FACE('',(#836),#4608,.F.);
#4848=ADVANCED_FACE('',(#837),#567,.T.);
#4849=ADVANCED_FACE('',(#838,#416),#568,.F.);
#4850=ADVANCED_FACE('',(#839),#4609,.T.);
#4851=ADVANCED_FACE('',(#840,#417),#569,.T.);
#4852=ADVANCED_FACE('',(#841),#131,.F.);
#4853=ADVANCED_FACE('',(#842),#116,.F.);
#4854=ADVANCED_FACE('',(#843),#4610,.F.);
#4855=ADVANCED_FACE('',(#844),#117,.F.);
#4856=ADVANCED_FACE('',(#845),#4611,.T.);
#4857=ADVANCED_FACE('',(#846),#4612,.T.);
#4858=ADVANCED_FACE('',(#847,#418),#570,.F.);
#4859=ADVANCED_FACE('',(#848,#419),#571,.F.);
#4860=ADVANCED_FACE('',(#849),#317,.T.);
#4861=ADVANCED_FACE('',(#850),#118,.T.);
#4862=ADVANCED_FACE('',(#851),#4613,.F.);
#4863=ADVANCED_FACE('',(#852),#132,.F.);
#4864=ADVANCED_FACE('',(#853),#4614,.F.);
#4865=ADVANCED_FACE('',(#854),#119,.T.);
#4866=ADVANCED_FACE('',(#855),#4615,.T.);
#4867=ADVANCED_FACE('',(#856,#420),#572,.F.);
#4868=ADVANCED_FACE('',(#857,#421),#573,.F.);
#4869=ADVANCED_FACE('',(#858),#318,.T.);
#4870=ADVANCED_FACE('',(#859),#319,.T.);
#4871=ADVANCED_FACE('',(#860),#320,.T.);
#4872=ADVANCED_FACE('',(#861),#321,.T.);
#4873=ADVANCED_FACE('',(#862),#322,.T.);
#4874=ADVANCED_FACE('',(#863),#323,.T.);
#4875=ADVANCED_FACE('',(#864),#324,.T.);
#4876=ADVANCED_FACE('',(#865),#133,.T.);
#4877=ADVANCED_FACE('',(#866,#422,#423),#325,.F.);
#4878=ADVANCED_FACE('',(#867,#424),#574,.T.);
#4879=ADVANCED_FACE('',(#868,#425),#575,.T.);
#4880=ADVANCED_FACE('',(#869),#134,.T.);
#4881=ADVANCED_FACE('',(#870,#426,#427),#326,.F.);
#4882=ADVANCED_FACE('',(#871,#428),#576,.T.);
#4883=ADVANCED_FACE('',(#872,#429),#577,.T.);
#4884=ADVANCED_FACE('',(#873),#135,.T.);
#4885=ADVANCED_FACE('',(#874,#430,#431),#327,.F.);
#4886=ADVANCED_FACE('',(#875,#432),#578,.T.);
#4887=ADVANCED_FACE('',(#876,#433),#579,.T.);
#4888=ADVANCED_FACE('',(#877),#136,.T.);
#4889=ADVANCED_FACE('',(#878,#434,#435),#328,.F.);
#4890=ADVANCED_FACE('',(#879,#436),#580,.T.);
#4891=ADVANCED_FACE('',(#880,#437),#581,.T.);
#4892=ADVANCED_FACE('',(#881),#137,.T.);
#4893=ADVANCED_FACE('',(#882,#438,#439),#329,.F.);
#4894=ADVANCED_FACE('',(#883,#440),#582,.T.);
#4895=ADVANCED_FACE('',(#884,#441),#583,.T.);
#4896=ADVANCED_FACE('',(#885),#138,.T.);
#4897=ADVANCED_FACE('',(#886,#442,#443),#330,.F.);
#4898=ADVANCED_FACE('',(#887,#444),#584,.T.);
#4899=ADVANCED_FACE('',(#888,#445),#585,.T.);
#4900=ADVANCED_FACE('',(#889),#139,.T.);
#4901=ADVANCED_FACE('',(#890,#446,#447),#331,.F.);
#4902=ADVANCED_FACE('',(#891,#448),#586,.T.);
#4903=ADVANCED_FACE('',(#892,#449),#587,.T.);
#4904=ADVANCED_FACE('',(#893),#140,.T.);
#4905=ADVANCED_FACE('',(#894,#450,#451),#332,.F.);
#4906=ADVANCED_FACE('',(#895,#452),#588,.T.);
#4907=ADVANCED_FACE('',(#896,#453),#589,.T.);
#4908=ADVANCED_FACE('',(#897),#4616,.F.);
#4909=ADVANCED_FACE('',(#898),#4617,.T.);
#4910=ADVANCED_FACE('',(#899,#454),#590,.T.);
#4911=ADVANCED_FACE('',(#900,#455),#591,.F.);
#4912=ADVANCED_FACE('',(#901),#141,.T.);
#4913=ADVANCED_FACE('',(#902),#142,.T.);
#4914=ADVANCED_FACE('',(#903),#4618,.T.);
#4915=ADVANCED_FACE('',(#904),#120,.T.);
#4916=ADVANCED_FACE('',(#905),#121,.F.);
#4917=ADVANCED_FACE('',(#906),#4619,.F.);
#4918=ADVANCED_FACE('',(#907,#456),#592,.F.);
#4919=ADVANCED_FACE('',(#908,#457),#593,.F.);
#4920=ADVANCED_FACE('',(#909),#143,.T.);
#4921=ADVANCED_FACE('',(#910),#144,.T.);
#4922=ADVANCED_FACE('',(#911),#4620,.F.);
#4923=ADVANCED_FACE('',(#912),#122,.F.);
#4924=ADVANCED_FACE('',(#913),#123,.T.);
#4925=ADVANCED_FACE('',(#914),#4621,.T.);
#4926=ADVANCED_FACE('',(#915,#458),#594,.F.);
#4927=ADVANCED_FACE('',(#916,#459),#595,.F.);
#4928=ADVANCED_FACE('',(#917),#4622,.F.);
#4929=ADVANCED_FACE('',(#918),#4623,.F.);
#4930=ADVANCED_FACE('',(#919),#4624,.F.);
#4931=ADVANCED_FACE('',(#920),#4625,.F.);
#4932=ADVANCED_FACE('',(#921),#4626,.F.);
#4933=ADVANCED_FACE('',(#922),#4627,.F.);
#4934=ADVANCED_FACE('',(#923),#4628,.F.);
#4935=ADVANCED_FACE('',(#924),#4629,.F.);
#4936=ADVANCED_FACE('',(#925),#596,.F.);
#4937=ADVANCED_FACE('',(#926),#597,.F.);
#4938=ADVANCED_FACE('',(#927),#598,.F.);
#4939=ADVANCED_FACE('',(#928,#460,#461),#599,.T.);
#4940=ADVANCED_FACE('',(#929),#600,.T.);
#4941=ADVANCED_FACE('',(#930,#462,#463,#464),#601,.T.);
#4942=ADVANCED_FACE('',(#931),#602,.T.);
#4943=ADVANCED_FACE('',(#932),#603,.T.);
#4944=ADVANCED_FACE('',(#933),#604,.T.);
#4945=ADVANCED_FACE('',(#934,#465,#466,#467),#605,.T.);
#4946=ADVANCED_FACE('',(#935,#468,#469),#606,.T.);
#4947=ADVANCED_FACE('',(#936),#607,.T.);
#4948=ADVANCED_FACE('',(#937),#608,.T.);
#4949=ADVANCED_FACE('',(#938),#609,.T.);
#4950=ADVANCED_FACE('',(#939,#470,#471),#610,.T.);
#4951=ADVANCED_FACE('',(#940),#611,.T.);
#4952=ADVANCED_FACE('',(#941),#612,.F.);
#4953=ADVANCED_FACE('',(#942),#613,.F.);
#4954=ADVANCED_FACE('',(#943),#614,.F.);
#4955=ADVANCED_FACE('',(#944,#472,#473),#615,.T.);
#4956=ADVANCED_FACE('',(#945,#474,#475,#476,#477),#4630,.F.);
#4957=ADVANCED_FACE('',(#946,#478,#479,#480,#481),#4631,.F.);
#4958=ADVANCED_FACE('',(#947),#4632,.F.);
#4959=ADVANCED_FACE('',(#948),#616,.T.);
#4960=ADVANCED_FACE('',(#949),#617,.T.);
#4961=ADVANCED_FACE('',(#950),#618,.T.);
#4962=ADVANCED_FACE('',(#951),#619,.T.);
#4963=ADVANCED_FACE('',(#952),#620,.T.);
#4964=ADVANCED_FACE('',(#953),#621,.T.);
#4965=CLOSED_SHELL('',(#4633,#4634,#4635,#4636,#4637,#4638,#4639,#4640,
#4641,#4642,#4643,#4644,#4645,#4646,#4647,#4648,#4649,#4650,#4651,#4652,
#4653,#4654,#4655,#4656,#4657,#4658,#4659,#4660,#4661,#4662,#4663,#4664,
#4665,#4666,#4667,#4668,#4669,#4670,#4671,#4672,#4673,#4674,#4675,#4676,
#4677));
#4966=CLOSED_SHELL('',(#4678,#4679,#4680,#4681,#4682,#4683,#4684,#4685,
#4686,#4687,#4688,#4689,#4690,#4691,#4692,#4693,#4694,#4695,#4696,#4697,
#4698,#4699,#4700,#4701,#4702,#4703,#4704,#4705,#4706,#4707,#4708,#4709,
#4710,#4711,#4712,#4713,#4714,#4715,#4716,#4717,#4718,#4719));
#4967=CLOSED_SHELL('',(#4720,#4721,#4722,#4723,#4724,#4725,#4726,#4727));
#4968=CLOSED_SHELL('',(#4728));
#4969=CLOSED_SHELL('',(#4729,#4730,#4731,#4732,#4733,#4734,#4735,#4736));
#4970=CLOSED_SHELL('',(#4737));
#4971=CLOSED_SHELL('',(#4738));
#4972=CLOSED_SHELL('',(#4739));
#4973=CLOSED_SHELL('',(#4740));
#4974=CLOSED_SHELL('',(#4741));
#4975=CLOSED_SHELL('',(#4742));
#4976=CLOSED_SHELL('',(#4743));
#4977=CLOSED_SHELL('',(#4744));
#4978=CLOSED_SHELL('',(#4745));
#4979=CLOSED_SHELL('',(#4746,#4747,#4748,#4749));
#4980=CLOSED_SHELL('',(#4750,#4751,#4752,#4753));
#4981=CLOSED_SHELL('',(#4754,#4755,#4756,#4757));
#4982=CLOSED_SHELL('',(#4758,#4759,#4760,#4761));
#4983=CLOSED_SHELL('',(#4762,#4763,#4764,#4765));
#4984=CLOSED_SHELL('',(#4766,#4767,#4768,#4769));
#4985=CLOSED_SHELL('',(#4770,#4771,#4772,#4773));
#4986=CLOSED_SHELL('',(#4774,#4775,#4776,#4777));
#4987=CLOSED_SHELL('',(#4778,#4779,#4780,#4781));
#4988=CLOSED_SHELL('',(#4782,#4783,#4784,#4785));
#4989=CLOSED_SHELL('',(#4786,#4787,#4788,#4789));
#4990=CLOSED_SHELL('',(#4790,#4791,#4792,#4793));
#4991=CLOSED_SHELL('',(#4794,#4795,#4796,#4797));
#4992=CLOSED_SHELL('',(#4798));
#4993=CLOSED_SHELL('',(#4799));
#4994=CLOSED_SHELL('',(#4800,#4801,#4802,#4803,#4804,#4805,#4806,#4807));
#4995=CLOSED_SHELL('',(#4808,#4809,#4810,#4811,#4812,#4813,#4814,#4815));
#4996=CLOSED_SHELL('',(#4816,#4817,#4818,#4819,#4820,#4821,#4822,#4823,
#4824,#4825,#4826,#4827,#4828,#4829,#4830,#4831,#4832,#4833,#4834));
#4997=CLOSED_SHELL('',(#4835,#4836,#4837,#4838,#4839,#4840,#4841));
#4998=CLOSED_SHELL('',(#4842,#4843,#4844));
#4999=CLOSED_SHELL('',(#4845,#4846,#4847,#4848,#4849,#4850,#4851));
#5000=CLOSED_SHELL('',(#4852,#4853,#4854,#4855,#4856,#4857,#4858,#4859));
#5001=CLOSED_SHELL('',(#4860));
#5002=CLOSED_SHELL('',(#4861,#4862,#4863,#4864,#4865,#4866,#4867,#4868));
#5003=CLOSED_SHELL('',(#4869));
#5004=CLOSED_SHELL('',(#4870));
#5005=CLOSED_SHELL('',(#4871));
#5006=CLOSED_SHELL('',(#4872));
#5007=CLOSED_SHELL('',(#4873));
#5008=CLOSED_SHELL('',(#4874));
#5009=CLOSED_SHELL('',(#4875));
#5010=CLOSED_SHELL('',(#4876,#4877,#4878,#4879));
#5011=CLOSED_SHELL('',(#4880,#4881,#4882,#4883));
#5012=CLOSED_SHELL('',(#4884,#4885,#4886,#4887));
#5013=CLOSED_SHELL('',(#4888,#4889,#4890,#4891));
#5014=CLOSED_SHELL('',(#4892,#4893,#4894,#4895));
#5015=CLOSED_SHELL('',(#4896,#4897,#4898,#4899));
#5016=CLOSED_SHELL('',(#4900,#4901,#4902,#4903));
#5017=CLOSED_SHELL('',(#4904,#4905,#4906,#4907));
#5018=CLOSED_SHELL('',(#4908,#4909,#4910,#4911));
#5019=CLOSED_SHELL('',(#4912,#4913,#4914,#4915,#4916,#4917,#4918,#4919));
#5020=CLOSED_SHELL('',(#4920,#4921,#4922,#4923,#4924,#4925,#4926,#4927));
#5021=CLOSED_SHELL('',(#4928,#4929,#4930,#4931,#4932,#4933,#4934,#4935,
#4936,#4937,#4938,#4939,#4940,#4941,#4942,#4943,#4944,#4945,#4946,#4947,
#4948,#4949,#4950,#4951,#4952,#4953,#4954,#4955,#4956,#4957,#4958,#4959,
#4960,#4961,#4962,#4963,#4964));
#5022=DERIVED_UNIT_ELEMENT(#5040,1.);
#5023=DERIVED_UNIT_ELEMENT(#9498,-3.);
#5024=DERIVED_UNIT_ELEMENT(#5040,1.);
#5025=DERIVED_UNIT_ELEMENT(#9498,-3.);
#5026=DERIVED_UNIT_ELEMENT(#5040,1.);
#5027=DERIVED_UNIT_ELEMENT(#9498,-3.);
#5028=DERIVED_UNIT_ELEMENT(#5040,1.);
#5029=DERIVED_UNIT_ELEMENT(#9498,-3.);
#5030=DERIVED_UNIT_ELEMENT(#5040,1.);
#5031=DERIVED_UNIT_ELEMENT(#9498,-3.);
#5032=DERIVED_UNIT_ELEMENT(#5040,1.);
#5033=DERIVED_UNIT_ELEMENT(#9498,-3.);
#5034=DERIVED_UNIT_ELEMENT(#5040,1.);
#5035=DERIVED_UNIT_ELEMENT(#9498,-3.);
#5036=DERIVED_UNIT_ELEMENT(#5040,1.);
#5037=DERIVED_UNIT_ELEMENT(#9498,-3.);
#5038=DERIVED_UNIT_ELEMENT(#5040,1.);
#5039=DERIVED_UNIT_ELEMENT(#9498,-3.);
#5040=(
MASS_UNIT()
NAMED_UNIT(*)
SI_UNIT(.KILO.,.GRAM.)
);
#5041=DERIVED_UNIT((#5022,#5023));
#5042=DERIVED_UNIT((#5024,#5025));
#5043=DERIVED_UNIT((#5026,#5027));
#5044=DERIVED_UNIT((#5028,#5029));
#5045=DERIVED_UNIT((#5030,#5031));
#5046=DERIVED_UNIT((#5032,#5033));
#5047=DERIVED_UNIT((#5034,#5035));
#5048=DERIVED_UNIT((#5036,#5037));
#5049=DERIVED_UNIT((#5038,#5039));
#5050=MEASURE_REPRESENTATION_ITEM('density measure',
POSITIVE_RATIO_MEASURE(7850.),#5041);
#5051=MEASURE_REPRESENTATION_ITEM('density measure',
POSITIVE_RATIO_MEASURE(7850.),#5042);
#5052=MEASURE_REPRESENTATION_ITEM('density measure',
POSITIVE_RATIO_MEASURE(7850.),#5043);
#5053=MEASURE_REPRESENTATION_ITEM('density measure',
POSITIVE_RATIO_MEASURE(7750.),#5044);
#5054=MEASURE_REPRESENTATION_ITEM('density measure',
POSITIVE_RATIO_MEASURE(7850.),#5045);
#5055=MEASURE_REPRESENTATION_ITEM('density measure',
POSITIVE_RATIO_MEASURE(7850.),#5046);
#5056=MEASURE_REPRESENTATION_ITEM('density measure',
POSITIVE_RATIO_MEASURE(7850.),#5047);
#5057=MEASURE_REPRESENTATION_ITEM('density measure',
POSITIVE_RATIO_MEASURE(7850.),#5048);
#5058=MEASURE_REPRESENTATION_ITEM('density measure',
POSITIVE_RATIO_MEASURE(7850.),#5049);
#5059=PROPERTY_DEFINITION_REPRESENTATION(#5104,#5077);
#5060=PROPERTY_DEFINITION_REPRESENTATION(#5105,#5078);
#5061=PROPERTY_DEFINITION_REPRESENTATION(#5106,#5079);
#5062=PROPERTY_DEFINITION_REPRESENTATION(#5107,#5080);
#5063=PROPERTY_DEFINITION_REPRESENTATION(#5108,#5081);
#5064=PROPERTY_DEFINITION_REPRESENTATION(#5109,#5082);
#5065=PROPERTY_DEFINITION_REPRESENTATION(#5110,#5083);
#5066=PROPERTY_DEFINITION_REPRESENTATION(#5111,#5084);
#5067=PROPERTY_DEFINITION_REPRESENTATION(#5112,#5085);
#5068=PROPERTY_DEFINITION_REPRESENTATION(#5113,#5086);
#5069=PROPERTY_DEFINITION_REPRESENTATION(#5114,#5087);
#5070=PROPERTY_DEFINITION_REPRESENTATION(#5115,#5088);
#5071=PROPERTY_DEFINITION_REPRESENTATION(#5116,#5089);
#5072=PROPERTY_DEFINITION_REPRESENTATION(#5117,#5090);
#5073=PROPERTY_DEFINITION_REPRESENTATION(#5118,#5091);
#5074=PROPERTY_DEFINITION_REPRESENTATION(#5119,#5092);
#5075=PROPERTY_DEFINITION_REPRESENTATION(#5120,#5093);
#5076=PROPERTY_DEFINITION_REPRESENTATION(#5121,#5094);
#5077=REPRESENTATION('material name',(#5095),#9487);
#5078=REPRESENTATION('density',(#5050),#9487);
#5079=REPRESENTATION('material name',(#5096),#9488);
#5080=REPRESENTATION('density',(#5051),#9488);
#5081=REPRESENTATION('material name',(#5097),#9489);
#5082=REPRESENTATION('density',(#5052),#9489);
#5083=REPRESENTATION('material name',(#5098),#9490);
#5084=REPRESENTATION('density',(#5053),#9490);
#5085=REPRESENTATION('material name',(#5099),#9491);
#5086=REPRESENTATION('density',(#5054),#9491);
#5087=REPRESENTATION('material name',(#5100),#9492);
#5088=REPRESENTATION('density',(#5055),#9492);
#5089=REPRESENTATION('material name',(#5101),#9493);
#5090=REPRESENTATION('density',(#5056),#9493);
#5091=REPRESENTATION('material name',(#5102),#9494);
#5092=REPRESENTATION('density',(#5057),#9494);
#5093=REPRESENTATION('material name',(#5103),#9495);
#5094=REPRESENTATION('density',(#5058),#9495);
#5095=DESCRIPTIVE_REPRESENTATION_ITEM('Steel','Steel');
#5096=DESCRIPTIVE_REPRESENTATION_ITEM('Steel','Steel');
#5097=DESCRIPTIVE_REPRESENTATION_ITEM('Steel','Steel');
#5098=DESCRIPTIVE_REPRESENTATION_ITEM('Steel Grade 2, Plain',
'Steel Grade 2, Plain');
#5099=DESCRIPTIVE_REPRESENTATION_ITEM('Steel','Steel');
#5100=DESCRIPTIVE_REPRESENTATION_ITEM('Steel','Steel');
#5101=DESCRIPTIVE_REPRESENTATION_ITEM('Steel','Steel');
#5102=DESCRIPTIVE_REPRESENTATION_ITEM('Steel','Steel');
#5103=DESCRIPTIVE_REPRESENTATION_ITEM('Steel','Steel');
#5104=PROPERTY_DEFINITION('material property','material name',#9550);
#5105=PROPERTY_DEFINITION('material property','density of part',#9550);
#5106=PROPERTY_DEFINITION('material property','material name',#9551);
#5107=PROPERTY_DEFINITION('material property','density of part',#9551);
#5108=PROPERTY_DEFINITION('material property','material name',#9552);
#5109=PROPERTY_DEFINITION('material property','density of part',#9552);
#5110=PROPERTY_DEFINITION('material property','material name',#9553);
#5111=PROPERTY_DEFINITION('material property','density of part',#9553);
#5112=PROPERTY_DEFINITION('material property','material name',#9554);
#5113=PROPERTY_DEFINITION('material property','density of part',#9554);
#5114=PROPERTY_DEFINITION('material property','material name',#9555);
#5115=PROPERTY_DEFINITION('material property','density of part',#9555);
#5116=PROPERTY_DEFINITION('material property','material name',#9556);
#5117=PROPERTY_DEFINITION('material property','density of part',#9556);
#5118=PROPERTY_DEFINITION('material property','material name',#9557);
#5119=PROPERTY_DEFINITION('material property','density of part',#9557);
#5120=PROPERTY_DEFINITION('material property','material name',#9558);
#5121=PROPERTY_DEFINITION('material property','density of part',#9558);
#5122=AXIS2_PLACEMENT_3D('',#7471,#5826,#5827);
#5123=AXIS2_PLACEMENT_3D('',#7472,#5828,#5829);
#5124=AXIS2_PLACEMENT_3D('',#7473,#5830,#5831);
#5125=AXIS2_PLACEMENT_3D('',#7475,#5832,#5833);
#5126=AXIS2_PLACEMENT_3D('',#7478,#5835,#5836);
#5127=AXIS2_PLACEMENT_3D('',#7479,#5837,#5838);
#5128=AXIS2_PLACEMENT_3D('',#7481,#5839,#5840);
#5129=AXIS2_PLACEMENT_3D('',#7482,#5841,#5842);
#5130=AXIS2_PLACEMENT_3D('',#7484,#5843,#5844);
#5131=AXIS2_PLACEMENT_3D('',#7487,#5846,#5847);
#5132=AXIS2_PLACEMENT_3D('',#7488,#5848,#5849);
#5133=AXIS2_PLACEMENT_3D('',#7489,#5850,#5851);
#5134=AXIS2_PLACEMENT_3D('',#7491,#5852,#5853);
#5135=AXIS2_PLACEMENT_3D('',#7494,#5855,#5856);
#5136=AXIS2_PLACEMENT_3D('',#7495,#5857,#5858);
#5137=AXIS2_PLACEMENT_3D('',#7496,#5859,#5860);
#5138=AXIS2_PLACEMENT_3D('',#7498,#5861,#5862);
#5139=AXIS2_PLACEMENT_3D('',#7501,#5864,#5865);
#5140=AXIS2_PLACEMENT_3D('',#7502,#5866,#5867);
#5141=AXIS2_PLACEMENT_3D('',#7504,#5868,#5869);
#5142=AXIS2_PLACEMENT_3D('',#7505,#5870,#5871);
#5143=AXIS2_PLACEMENT_3D('',#7508,#5873,#5874);
#5144=AXIS2_PLACEMENT_3D('',#7509,#5875,#5876);
#5145=AXIS2_PLACEMENT_3D('',#7511,#5877,#5878);
#5146=AXIS2_PLACEMENT_3D('',#7514,#5880,#5881);
#5147=AXIS2_PLACEMENT_3D('',#7515,#5882,#5883);
#5148=AXIS2_PLACEMENT_3D('',#7516,#5884,#5885);
#5149=AXIS2_PLACEMENT_3D('',#7519,#5887,#5888);
#5150=AXIS2_PLACEMENT_3D('',#7520,#5889,#5890);
#5151=AXIS2_PLACEMENT_3D('',#7525,#5892,#5893);
#5152=AXIS2_PLACEMENT_3D('',#7528,#5895,#5896);
#5153=AXIS2_PLACEMENT_3D('',#7529,#5897,#5898);
#5154=AXIS2_PLACEMENT_3D('',#7543,#5906,#5907);
#5155=AXIS2_PLACEMENT_3D('',#7551,#5911,#5912);
#5156=AXIS2_PLACEMENT_3D('',#7554,#5914,#5915);
#5157=AXIS2_PLACEMENT_3D('',#7555,#5916,#5917);
#5158=AXIS2_PLACEMENT_3D('',#7558,#5919,#5920);
#5159=AXIS2_PLACEMENT_3D('',#7559,#5921,#5922);
#5160=AXIS2_PLACEMENT_3D('',#7561,#5923,#5924);
#5161=AXIS2_PLACEMENT_3D('',#7565,#5926,#5927);
#5162=AXIS2_PLACEMENT_3D('',#7569,#5930,#5931);
#5163=AXIS2_PLACEMENT_3D('',#7572,#5933,#5934);
#5164=AXIS2_PLACEMENT_3D('',#7573,#5935,#5936);
#5165=AXIS2_PLACEMENT_3D('',#7577,#5939,#5940);
#5166=AXIS2_PLACEMENT_3D('',#7580,#5942,#5943);
#5167=AXIS2_PLACEMENT_3D('',#7581,#5944,#5945);
#5168=AXIS2_PLACEMENT_3D('',#7585,#5947,#5948);
#5169=AXIS2_PLACEMENT_3D('',#7587,#5950,#5951);
#5170=AXIS2_PLACEMENT_3D('',#7590,#5952,#5953);
#5171=AXIS2_PLACEMENT_3D('',#7592,#5954,#5955);
#5172=AXIS2_PLACEMENT_3D('',#7593,#5956,#5957);
#5173=AXIS2_PLACEMENT_3D('',#7594,#5958,#5959);
#5174=AXIS2_PLACEMENT_3D('',#7596,#5960,#5961);
#5175=AXIS2_PLACEMENT_3D('',#7597,#5962,#5963);
#5176=AXIS2_PLACEMENT_3D('',#7598,#5964,#5965);
#5177=AXIS2_PLACEMENT_3D('',#7601,#5968,#5969);
#5178=AXIS2_PLACEMENT_3D('',#7604,#5970,#5971);
#5179=AXIS2_PLACEMENT_3D('',#7605,#5972,#5973);
#5180=AXIS2_PLACEMENT_3D('',#7606,#5974,#5975);
#5181=AXIS2_PLACEMENT_3D('',#7607,#5976,#5977);
#5182=AXIS2_PLACEMENT_3D('',#7609,#5978,#5979);
#5183=AXIS2_PLACEMENT_3D('',#7610,#5980,#5981);
#5184=AXIS2_PLACEMENT_3D('',#7611,#5982,#5983);
#5185=AXIS2_PLACEMENT_3D('',#7616,#5986,#5987);
#5186=AXIS2_PLACEMENT_3D('',#7617,#5988,#5989);
#5187=AXIS2_PLACEMENT_3D('',#7619,#5990,#5991);
#5188=AXIS2_PLACEMENT_3D('',#7621,#5992,#5993);
#5189=AXIS2_PLACEMENT_3D('',#7622,#5994,#5995);
#5190=AXIS2_PLACEMENT_3D('',#7623,#5996,#5997);
#5191=AXIS2_PLACEMENT_3D('',#7625,#5999,#6000);
#5192=AXIS2_PLACEMENT_3D('',#7628,#6003,#6004);
#5193=AXIS2_PLACEMENT_3D('',#7630,#6005,#6006);
#5194=AXIS2_PLACEMENT_3D('',#7631,#6007,#6008);
#5195=AXIS2_PLACEMENT_3D('',#7632,#6009,#6010);
#5196=AXIS2_PLACEMENT_3D('',#7635,#6012,#6013);
#5197=AXIS2_PLACEMENT_3D('',#7636,#6014,#6015);
#5198=AXIS2_PLACEMENT_3D('',#7638,#6017,#6018);
#5199=AXIS2_PLACEMENT_3D('',#7640,#6020,#6021);
#5200=AXIS2_PLACEMENT_3D('',#7642,#6023,#6024);
#5201=AXIS2_PLACEMENT_3D('',#7645,#6027,#6028);
#5202=AXIS2_PLACEMENT_3D('',#7648,#6031,#6032);
#5203=AXIS2_PLACEMENT_3D('',#7650,#6034,#6035);
#5204=AXIS2_PLACEMENT_3D('',#7651,#6036,#6037);
#5205=AXIS2_PLACEMENT_3D('',#7653,#6038,#6039);
#5206=AXIS2_PLACEMENT_3D('',#7654,#6040,#6041);
#5207=AXIS2_PLACEMENT_3D('',#7655,#6042,#6043);
#5208=AXIS2_PLACEMENT_3D('',#7656,#6044,#6045);
#5209=AXIS2_PLACEMENT_3D('',#7657,#6046,#6047);
#5210=AXIS2_PLACEMENT_3D('',#7659,#6048,#6049);
#5211=AXIS2_PLACEMENT_3D('',#7660,#6050,#6051);
#5212=AXIS2_PLACEMENT_3D('',#7662,#6053,#6054);
#5213=AXIS2_PLACEMENT_3D('',#7663,#6055,#6056);
#5214=AXIS2_PLACEMENT_3D('',#7664,#6057,#6058);
#5215=AXIS2_PLACEMENT_3D('',#7666,#6059,#6060);
#5216=AXIS2_PLACEMENT_3D('',#7669,#6062,#6063);
#5217=AXIS2_PLACEMENT_3D('',#7670,#6064,#6065);
#5218=AXIS2_PLACEMENT_3D('',#7672,#6066,#6067);
#5219=AXIS2_PLACEMENT_3D('',#7673,#6068,#6069);
#5220=AXIS2_PLACEMENT_3D('',#7675,#6070,#6071);
#5221=AXIS2_PLACEMENT_3D('',#7678,#6073,#6074);
#5222=AXIS2_PLACEMENT_3D('',#7679,#6075,#6076);
#5223=AXIS2_PLACEMENT_3D('',#7680,#6077,#6078);
#5224=AXIS2_PLACEMENT_3D('',#7682,#6079,#6080);
#5225=AXIS2_PLACEMENT_3D('',#7685,#6082,#6083);
#5226=AXIS2_PLACEMENT_3D('',#7686,#6084,#6085);
#5227=AXIS2_PLACEMENT_3D('',#7687,#6086,#6087);
#5228=AXIS2_PLACEMENT_3D('',#7689,#6088,#6089);
#5229=AXIS2_PLACEMENT_3D('',#7692,#6091,#6092);
#5230=AXIS2_PLACEMENT_3D('',#7693,#6093,#6094);
#5231=AXIS2_PLACEMENT_3D('',#7695,#6095,#6096);
#5232=AXIS2_PLACEMENT_3D('',#7696,#6097,#6098);
#5233=AXIS2_PLACEMENT_3D('',#7698,#6099,#6100);
#5234=AXIS2_PLACEMENT_3D('',#7701,#6102,#6103);
#5235=AXIS2_PLACEMENT_3D('',#7702,#6104,#6105);
#5236=AXIS2_PLACEMENT_3D('',#7704,#6106,#6107);
#5237=AXIS2_PLACEMENT_3D('',#7705,#6108,#6109);
#5238=AXIS2_PLACEMENT_3D('',#7707,#6111,#6112);
#5239=AXIS2_PLACEMENT_3D('',#7710,#6114,#6115);
#5240=AXIS2_PLACEMENT_3D('',#7711,#6116,#6117);
#5241=AXIS2_PLACEMENT_3D('',#7714,#6118,#6119);
#5242=AXIS2_PLACEMENT_3D('',#7716,#6120,#6121);
#5243=AXIS2_PLACEMENT_3D('',#7717,#6122,#6123);
#5244=AXIS2_PLACEMENT_3D('',#7718,#6124,#6125);
#5245=AXIS2_PLACEMENT_3D('',#7721,#6126,#6127);
#5246=AXIS2_PLACEMENT_3D('',#7723,#6128,#6129);
#5247=AXIS2_PLACEMENT_3D('',#7724,#6130,#6131);
#5248=AXIS2_PLACEMENT_3D('',#7725,#6132,#6133);
#5249=AXIS2_PLACEMENT_3D('',#7728,#6134,#6135);
#5250=AXIS2_PLACEMENT_3D('',#7730,#6136,#6137);
#5251=AXIS2_PLACEMENT_3D('',#7731,#6138,#6139);
#5252=AXIS2_PLACEMENT_3D('',#7732,#6140,#6141);
#5253=AXIS2_PLACEMENT_3D('',#7735,#6142,#6143);
#5254=AXIS2_PLACEMENT_3D('',#7737,#6144,#6145);
#5255=AXIS2_PLACEMENT_3D('',#7738,#6146,#6147);
#5256=AXIS2_PLACEMENT_3D('',#7739,#6148,#6149);
#5257=AXIS2_PLACEMENT_3D('',#7742,#6152,#6153);
#5258=AXIS2_PLACEMENT_3D('',#7745,#6154,#6155);
#5259=AXIS2_PLACEMENT_3D('',#7747,#6156,#6157);
#5260=AXIS2_PLACEMENT_3D('',#7748,#6158,#6159);
#5261=AXIS2_PLACEMENT_3D('',#7749,#6160,#6161);
#5262=AXIS2_PLACEMENT_3D('',#7752,#6162,#6163);
#5263=AXIS2_PLACEMENT_3D('',#7754,#6164,#6165);
#5264=AXIS2_PLACEMENT_3D('',#7755,#6166,#6167);
#5265=AXIS2_PLACEMENT_3D('',#7756,#6168,#6169);
#5266=AXIS2_PLACEMENT_3D('',#7759,#6172,#6173);
#5267=AXIS2_PLACEMENT_3D('',#7762,#6174,#6175);
#5268=AXIS2_PLACEMENT_3D('',#7764,#6176,#6177);
#5269=AXIS2_PLACEMENT_3D('',#7765,#6178,#6179);
#5270=AXIS2_PLACEMENT_3D('',#7766,#6180,#6181);
#5271=AXIS2_PLACEMENT_3D('',#7769,#6184,#6185);
#5272=AXIS2_PLACEMENT_3D('',#7772,#6188,#6189);
#5273=AXIS2_PLACEMENT_3D('',#7775,#6190,#6191);
#5274=AXIS2_PLACEMENT_3D('',#7777,#6192,#6193);
#5275=AXIS2_PLACEMENT_3D('',#7778,#6194,#6195);
#5276=AXIS2_PLACEMENT_3D('',#7779,#6196,#6197);
#5277=AXIS2_PLACEMENT_3D('',#7782,#6200,#6201);
#5278=AXIS2_PLACEMENT_3D('',#7785,#6204,#6205);
#5279=AXIS2_PLACEMENT_3D('',#7788,#6208,#6209);
#5280=AXIS2_PLACEMENT_3D('',#7791,#6212,#6213);
#5281=AXIS2_PLACEMENT_3D('',#7794,#6216,#6217);
#5282=AXIS2_PLACEMENT_3D('',#7797,#6220,#6221);
#5283=AXIS2_PLACEMENT_3D('',#7800,#6224,#6225);
#5284=AXIS2_PLACEMENT_3D('',#7803,#6228,#6229);
#5285=AXIS2_PLACEMENT_3D('',#7805,#6230,#6231);
#5286=AXIS2_PLACEMENT_3D('',#7807,#6232,#6233);
#5287=AXIS2_PLACEMENT_3D('',#7808,#6234,#6235);
#5288=AXIS2_PLACEMENT_3D('',#7809,#6236,#6237);
#5289=AXIS2_PLACEMENT_3D('',#7810,#6238,#6239);
#5290=AXIS2_PLACEMENT_3D('',#7811,#6240,#6241);
#5291=AXIS2_PLACEMENT_3D('',#7812,#6242,#6243);
#5292=AXIS2_PLACEMENT_3D('',#7813,#6244,#6245);
#5293=AXIS2_PLACEMENT_3D('',#7816,#6247,#6248);
#5294=AXIS2_PLACEMENT_3D('',#7817,#6249,#6250);
#5295=AXIS2_PLACEMENT_3D('',#7818,#6251,#6252);
#5296=AXIS2_PLACEMENT_3D('',#7821,#6254,#6255);
#5297=AXIS2_PLACEMENT_3D('',#7822,#6256,#6257);
#5298=AXIS2_PLACEMENT_3D('',#7823,#6258,#6259);
#5299=AXIS2_PLACEMENT_3D('',#7824,#6260,#6261);
#5300=AXIS2_PLACEMENT_3D('',#7826,#6262,#6263);
#5301=AXIS2_PLACEMENT_3D('',#7828,#6264,#6265);
#5302=AXIS2_PLACEMENT_3D('',#7829,#6266,#6267);
#5303=AXIS2_PLACEMENT_3D('',#7830,#6268,#6269);
#5304=AXIS2_PLACEMENT_3D('',#7832,#6270,#6271);
#5305=AXIS2_PLACEMENT_3D('',#7835,#6273,#6274);
#5306=AXIS2_PLACEMENT_3D('',#7836,#6275,#6276);
#5307=AXIS2_PLACEMENT_3D('',#7840,#6278,#6279);
#5308=AXIS2_PLACEMENT_3D('',#7841,#6280,#6281);
#5309=AXIS2_PLACEMENT_3D('',#7842,#6282,#6283);
#5310=AXIS2_PLACEMENT_3D('',#7845,#6285,#6286);
#5311=AXIS2_PLACEMENT_3D('',#7846,#6287,#6288);
#5312=AXIS2_PLACEMENT_3D('',#7848,#6289,#6290);
#5313=AXIS2_PLACEMENT_3D('',#7850,#6292,#6293);
#5314=AXIS2_PLACEMENT_3D('',#7853,#6295,#6296);
#5315=AXIS2_PLACEMENT_3D('',#7854,#6297,#6298);
#5316=AXIS2_PLACEMENT_3D('',#7855,#6299,#6300);
#5317=AXIS2_PLACEMENT_3D('',#7856,#6301,#6302);
#5318=AXIS2_PLACEMENT_3D('',#7859,#6303,#6304);
#5319=AXIS2_PLACEMENT_3D('',#7860,#6305,#6306);
#5320=AXIS2_PLACEMENT_3D('',#7862,#6307,#6308);
#5321=AXIS2_PLACEMENT_3D('',#7865,#6310,#6311);
#5322=AXIS2_PLACEMENT_3D('',#7866,#6312,#6313);
#5323=AXIS2_PLACEMENT_3D('',#7868,#6314,#6315);
#5324=AXIS2_PLACEMENT_3D('',#7871,#6317,#6318);
#5325=AXIS2_PLACEMENT_3D('',#7872,#6319,#6320);
#5326=AXIS2_PLACEMENT_3D('',#7874,#6321,#6322);
#5327=AXIS2_PLACEMENT_3D('',#7875,#6323,#6324);
#5328=AXIS2_PLACEMENT_3D('',#7876,#6325,#6326);
#5329=AXIS2_PLACEMENT_3D('',#7878,#6327,#6328);
#5330=AXIS2_PLACEMENT_3D('',#7880,#6330,#6331);
#5331=AXIS2_PLACEMENT_3D('',#7883,#6332,#6333);
#5332=AXIS2_PLACEMENT_3D('',#7884,#6334,#6335);
#5333=AXIS2_PLACEMENT_3D('',#7887,#6337,#6338);
#5334=AXIS2_PLACEMENT_3D('',#7888,#6339,#6340);
#5335=AXIS2_PLACEMENT_3D('',#7890,#6342,#6343);
#5336=AXIS2_PLACEMENT_3D('',#7891,#6344,#6345);
#5337=AXIS2_PLACEMENT_3D('',#7892,#6346,#6347);
#5338=AXIS2_PLACEMENT_3D('',#7895,#6348,#6349);
#5339=AXIS2_PLACEMENT_3D('',#7896,#6350,#6351);
#5340=AXIS2_PLACEMENT_3D('',#7899,#6352,#6353);
#5341=AXIS2_PLACEMENT_3D('',#7900,#6354,#6355);
#5342=AXIS2_PLACEMENT_3D('',#7903,#6356,#6357);
#5343=AXIS2_PLACEMENT_3D('',#7904,#6358,#6359);
#5344=AXIS2_PLACEMENT_3D('',#7907,#6360,#6361);
#5345=AXIS2_PLACEMENT_3D('',#7908,#6362,#6363);
#5346=AXIS2_PLACEMENT_3D('',#7911,#6364,#6365);
#5347=AXIS2_PLACEMENT_3D('',#7912,#6366,#6367);
#5348=AXIS2_PLACEMENT_3D('',#7915,#6368,#6369);
#5349=AXIS2_PLACEMENT_3D('',#7916,#6370,#6371);
#5350=AXIS2_PLACEMENT_3D('',#7919,#6372,#6373);
#5351=AXIS2_PLACEMENT_3D('',#7920,#6374,#6375);
#5352=AXIS2_PLACEMENT_3D('',#7923,#6376,#6377);
#5353=AXIS2_PLACEMENT_3D('',#7924,#6378,#6379);
#5354=AXIS2_PLACEMENT_3D('',#7927,#6380,#6381);
#5355=AXIS2_PLACEMENT_3D('',#7956,#6382,#6383);
#5356=AXIS2_PLACEMENT_3D('',#7958,#6384,#6385);
#5357=AXIS2_PLACEMENT_3D('',#7959,#6386,#6387);
#5358=AXIS2_PLACEMENT_3D('',#7960,#6388,#6389);
#5359=AXIS2_PLACEMENT_3D('',#7963,#6390,#6391);
#5360=AXIS2_PLACEMENT_3D('',#7965,#6392,#6393);
#5361=AXIS2_PLACEMENT_3D('',#7967,#6394,#6395);
#5362=AXIS2_PLACEMENT_3D('',#7968,#6396,#6397);
#5363=AXIS2_PLACEMENT_3D('',#7969,#6398,#6399);
#5364=AXIS2_PLACEMENT_3D('',#7998,#6400,#6401);
#5365=AXIS2_PLACEMENT_3D('',#8000,#6402,#6403);
#5366=AXIS2_PLACEMENT_3D('',#8001,#6404,#6405);
#5367=AXIS2_PLACEMENT_3D('',#8002,#6406,#6407);
#5368=AXIS2_PLACEMENT_3D('',#8005,#6408,#6409);
#5369=AXIS2_PLACEMENT_3D('',#8007,#6410,#6411);
#5370=AXIS2_PLACEMENT_3D('',#8009,#6412,#6413);
#5371=AXIS2_PLACEMENT_3D('',#8010,#6414,#6415);
#5372=AXIS2_PLACEMENT_3D('',#8011,#6416,#6417);
#5373=AXIS2_PLACEMENT_3D('',#8040,#6418,#6419);
#5374=AXIS2_PLACEMENT_3D('',#8042,#6420,#6421);
#5375=AXIS2_PLACEMENT_3D('',#8043,#6422,#6423);
#5376=AXIS2_PLACEMENT_3D('',#8044,#6424,#6425);
#5377=AXIS2_PLACEMENT_3D('',#8047,#6426,#6427);
#5378=AXIS2_PLACEMENT_3D('',#8049,#6428,#6429);
#5379=AXIS2_PLACEMENT_3D('',#8051,#6430,#6431);
#5380=AXIS2_PLACEMENT_3D('',#8052,#6432,#6433);
#5381=AXIS2_PLACEMENT_3D('',#8053,#6434,#6435);
#5382=AXIS2_PLACEMENT_3D('',#8082,#6436,#6437);
#5383=AXIS2_PLACEMENT_3D('',#8084,#6438,#6439);
#5384=AXIS2_PLACEMENT_3D('',#8085,#6440,#6441);
#5385=AXIS2_PLACEMENT_3D('',#8086,#6442,#6443);
#5386=AXIS2_PLACEMENT_3D('',#8089,#6444,#6445);
#5387=AXIS2_PLACEMENT_3D('',#8091,#6446,#6447);
#5388=AXIS2_PLACEMENT_3D('',#8093,#6448,#6449);
#5389=AXIS2_PLACEMENT_3D('',#8094,#6450,#6451);
#5390=AXIS2_PLACEMENT_3D('',#8095,#6452,#6453);
#5391=AXIS2_PLACEMENT_3D('',#8124,#6454,#6455);
#5392=AXIS2_PLACEMENT_3D('',#8126,#6456,#6457);
#5393=AXIS2_PLACEMENT_3D('',#8127,#6458,#6459);
#5394=AXIS2_PLACEMENT_3D('',#8128,#6460,#6461);
#5395=AXIS2_PLACEMENT_3D('',#8131,#6462,#6463);
#5396=AXIS2_PLACEMENT_3D('',#8133,#6464,#6465);
#5397=AXIS2_PLACEMENT_3D('',#8135,#6466,#6467);
#5398=AXIS2_PLACEMENT_3D('',#8136,#6468,#6469);
#5399=AXIS2_PLACEMENT_3D('',#8137,#6470,#6471);
#5400=AXIS2_PLACEMENT_3D('',#8166,#6472,#6473);
#5401=AXIS2_PLACEMENT_3D('',#8168,#6474,#6475);
#5402=AXIS2_PLACEMENT_3D('',#8169,#6476,#6477);
#5403=AXIS2_PLACEMENT_3D('',#8170,#6478,#6479);
#5404=AXIS2_PLACEMENT_3D('',#8173,#6480,#6481);
#5405=AXIS2_PLACEMENT_3D('',#8175,#6482,#6483);
#5406=AXIS2_PLACEMENT_3D('',#8177,#6484,#6485);
#5407=AXIS2_PLACEMENT_3D('',#8178,#6486,#6487);
#5408=AXIS2_PLACEMENT_3D('',#8179,#6488,#6489);
#5409=AXIS2_PLACEMENT_3D('',#8208,#6490,#6491);
#5410=AXIS2_PLACEMENT_3D('',#8210,#6492,#6493);
#5411=AXIS2_PLACEMENT_3D('',#8211,#6494,#6495);
#5412=AXIS2_PLACEMENT_3D('',#8212,#6496,#6497);
#5413=AXIS2_PLACEMENT_3D('',#8215,#6498,#6499);
#5414=AXIS2_PLACEMENT_3D('',#8217,#6500,#6501);
#5415=AXIS2_PLACEMENT_3D('',#8219,#6502,#6503);
#5416=AXIS2_PLACEMENT_3D('',#8220,#6504,#6505);
#5417=AXIS2_PLACEMENT_3D('',#8221,#6506,#6507);
#5418=AXIS2_PLACEMENT_3D('',#8250,#6508,#6509);
#5419=AXIS2_PLACEMENT_3D('',#8252,#6510,#6511);
#5420=AXIS2_PLACEMENT_3D('',#8253,#6512,#6513);
#5421=AXIS2_PLACEMENT_3D('',#8254,#6514,#6515);
#5422=AXIS2_PLACEMENT_3D('',#8257,#6516,#6517);
#5423=AXIS2_PLACEMENT_3D('',#8259,#6518,#6519);
#5424=AXIS2_PLACEMENT_3D('',#8261,#6520,#6521);
#5425=AXIS2_PLACEMENT_3D('',#8262,#6522,#6523);
#5426=AXIS2_PLACEMENT_3D('',#8263,#6524,#6525);
#5427=AXIS2_PLACEMENT_3D('',#8292,#6526,#6527);
#5428=AXIS2_PLACEMENT_3D('',#8294,#6528,#6529);
#5429=AXIS2_PLACEMENT_3D('',#8295,#6530,#6531);
#5430=AXIS2_PLACEMENT_3D('',#8296,#6532,#6533);
#5431=AXIS2_PLACEMENT_3D('',#8299,#6534,#6535);
#5432=AXIS2_PLACEMENT_3D('',#8301,#6536,#6537);
#5433=AXIS2_PLACEMENT_3D('',#8303,#6538,#6539);
#5434=AXIS2_PLACEMENT_3D('',#8304,#6540,#6541);
#5435=AXIS2_PLACEMENT_3D('',#8305,#6542,#6543);
#5436=AXIS2_PLACEMENT_3D('',#8334,#6544,#6545);
#5437=AXIS2_PLACEMENT_3D('',#8336,#6546,#6547);
#5438=AXIS2_PLACEMENT_3D('',#8337,#6548,#6549);
#5439=AXIS2_PLACEMENT_3D('',#8338,#6550,#6551);
#5440=AXIS2_PLACEMENT_3D('',#8341,#6552,#6553);
#5441=AXIS2_PLACEMENT_3D('',#8343,#6554,#6555);
#5442=AXIS2_PLACEMENT_3D('',#8345,#6556,#6557);
#5443=AXIS2_PLACEMENT_3D('',#8346,#6558,#6559);
#5444=AXIS2_PLACEMENT_3D('',#8347,#6560,#6561);
#5445=AXIS2_PLACEMENT_3D('',#8348,#6562,#6563);
#5446=AXIS2_PLACEMENT_3D('',#8350,#6564,#6565);
#5447=AXIS2_PLACEMENT_3D('',#8353,#6567,#6568);
#5448=AXIS2_PLACEMENT_3D('',#8354,#6569,#6570);
#5449=AXIS2_PLACEMENT_3D('',#8356,#6571,#6572);
#5450=AXIS2_PLACEMENT_3D('',#8359,#6574,#6575);
#5451=AXIS2_PLACEMENT_3D('',#8360,#6576,#6577);
#5452=AXIS2_PLACEMENT_3D('',#8361,#6578,#6579);
#5453=AXIS2_PLACEMENT_3D('',#8390,#6580,#6581);
#5454=AXIS2_PLACEMENT_3D('',#8392,#6582,#6583);
#5455=AXIS2_PLACEMENT_3D('',#8393,#6584,#6585);
#5456=AXIS2_PLACEMENT_3D('',#8394,#6586,#6587);
#5457=AXIS2_PLACEMENT_3D('',#8397,#6588,#6589);
#5458=AXIS2_PLACEMENT_3D('',#8399,#6590,#6591);
#5459=AXIS2_PLACEMENT_3D('',#8401,#6592,#6593);
#5460=AXIS2_PLACEMENT_3D('',#8402,#6594,#6595);
#5461=AXIS2_PLACEMENT_3D('',#8403,#6596,#6597);
#5462=AXIS2_PLACEMENT_3D('',#8432,#6598,#6599);
#5463=AXIS2_PLACEMENT_3D('',#8434,#6600,#6601);
#5464=AXIS2_PLACEMENT_3D('',#8435,#6602,#6603);
#5465=AXIS2_PLACEMENT_3D('',#8436,#6604,#6605);
#5466=AXIS2_PLACEMENT_3D('',#8439,#6606,#6607);
#5467=AXIS2_PLACEMENT_3D('',#8441,#6608,#6609);
#5468=AXIS2_PLACEMENT_3D('',#8443,#6610,#6611);
#5469=AXIS2_PLACEMENT_3D('',#8444,#6612,#6613);
#5470=AXIS2_PLACEMENT_3D('',#8445,#6614,#6615);
#5471=AXIS2_PLACEMENT_3D('',#8446,#6616,#6617);
#5472=AXIS2_PLACEMENT_3D('',#8449,#6618,#6619);
#5473=AXIS2_PLACEMENT_3D('',#8450,#6620,#6621);
#5474=AXIS2_PLACEMENT_3D('',#8453,#6622,#6623);
#5475=AXIS2_PLACEMENT_3D('',#8454,#6624,#6625);
#5476=AXIS2_PLACEMENT_3D('',#8456,#6626,#6627);
#5477=AXIS2_PLACEMENT_3D('',#8458,#6628,#6629);
#5478=AXIS2_PLACEMENT_3D('',#8460,#6630,#6631);
#5479=AXIS2_PLACEMENT_3D('',#8461,#6632,#6633);
#5480=AXIS2_PLACEMENT_3D('',#8462,#6634,#6635);
#5481=AXIS2_PLACEMENT_3D('',#8465,#6636,#6637);
#5482=AXIS2_PLACEMENT_3D('',#8467,#6638,#6639);
#5483=AXIS2_PLACEMENT_3D('',#8468,#6640,#6641);
#5484=AXIS2_PLACEMENT_3D('',#8469,#6642,#6643);
#5485=AXIS2_PLACEMENT_3D('',#8470,#6644,#6645);
#5486=AXIS2_PLACEMENT_3D('',#8473,#6646,#6647);
#5487=AXIS2_PLACEMENT_3D('',#8474,#6648,#6649);
#5488=AXIS2_PLACEMENT_3D('',#8476,#6651,#6652);
#5489=AXIS2_PLACEMENT_3D('',#8478,#6653,#6654);
#5490=AXIS2_PLACEMENT_3D('',#8480,#6656,#6657);
#5491=AXIS2_PLACEMENT_3D('',#8482,#6658,#6659);
#5492=AXIS2_PLACEMENT_3D('',#8485,#6661,#6662);
#5493=AXIS2_PLACEMENT_3D('',#8486,#6663,#6664);
#5494=AXIS2_PLACEMENT_3D('',#8488,#6666,#6667);
#5495=AXIS2_PLACEMENT_3D('',#8489,#6668,#6669);
#5496=AXIS2_PLACEMENT_3D('',#8490,#6670,#6671);
#5497=AXIS2_PLACEMENT_3D('',#8492,#6672,#6673);
#5498=AXIS2_PLACEMENT_3D('',#8494,#6674,#6675);
#5499=AXIS2_PLACEMENT_3D('',#8495,#6676,#6677);
#5500=AXIS2_PLACEMENT_3D('',#8496,#6678,#6679);
#5501=AXIS2_PLACEMENT_3D('',#8498,#6680,#6681);
#5502=AXIS2_PLACEMENT_3D('',#8500,#6682,#6683);
#5503=AXIS2_PLACEMENT_3D('',#8501,#6684,#6685);
#5504=AXIS2_PLACEMENT_3D('',#8502,#6686,#6687);
#5505=AXIS2_PLACEMENT_3D('',#8505,#6688,#6689);
#5506=AXIS2_PLACEMENT_3D('',#8506,#6690,#6691);
#5507=AXIS2_PLACEMENT_3D('',#8508,#6693,#6694);
#5508=AXIS2_PLACEMENT_3D('',#8510,#6695,#6696);
#5509=AXIS2_PLACEMENT_3D('',#8512,#6698,#6699);
#5510=AXIS2_PLACEMENT_3D('',#8514,#6700,#6701);
#5511=AXIS2_PLACEMENT_3D('',#8517,#6703,#6704);
#5512=AXIS2_PLACEMENT_3D('',#8518,#6705,#6706);
#5513=AXIS2_PLACEMENT_3D('',#8520,#6708,#6709);
#5514=AXIS2_PLACEMENT_3D('',#8521,#6710,#6711);
#5515=AXIS2_PLACEMENT_3D('',#8522,#6712,#6713);
#5516=AXIS2_PLACEMENT_3D('',#8523,#6714,#6715);
#5517=AXIS2_PLACEMENT_3D('',#8525,#6716,#6717);
#5518=AXIS2_PLACEMENT_3D('',#8528,#6719,#6720);
#5519=AXIS2_PLACEMENT_3D('',#8529,#6721,#6722);
#5520=AXIS2_PLACEMENT_3D('',#8531,#6723,#6724);
#5521=AXIS2_PLACEMENT_3D('',#8533,#6725,#6726);
#5522=AXIS2_PLACEMENT_3D('',#8534,#6727,#6728);
#5523=AXIS2_PLACEMENT_3D('',#8535,#6729,#6730);
#5524=AXIS2_PLACEMENT_3D('',#8548,#6737,#6738);
#5525=AXIS2_PLACEMENT_3D('',#8550,#6739,#6740);
#5526=AXIS2_PLACEMENT_3D('',#8552,#6742,#6743);
#5527=AXIS2_PLACEMENT_3D('',#8559,#6747,#6748);
#5528=AXIS2_PLACEMENT_3D('',#8563,#6751,#6752);
#5529=AXIS2_PLACEMENT_3D('',#8567,#6755,#6756);
#5530=AXIS2_PLACEMENT_3D('',#8571,#6759,#6760);
#5531=AXIS2_PLACEMENT_3D('',#8575,#6763,#6764);
#5532=AXIS2_PLACEMENT_3D('',#8577,#6766,#6767);
#5533=AXIS2_PLACEMENT_3D('',#8580,#6770,#6771);
#5534=AXIS2_PLACEMENT_3D('',#8582,#6773,#6774);
#5535=AXIS2_PLACEMENT_3D('',#8584,#6776,#6777);
#5536=AXIS2_PLACEMENT_3D('',#8586,#6779,#6780);
#5537=AXIS2_PLACEMENT_3D('',#8588,#6782,#6783);
#5538=AXIS2_PLACEMENT_3D('',#8589,#6784,#6785);
#5539=AXIS2_PLACEMENT_3D('',#8592,#6787,#6788);
#5540=AXIS2_PLACEMENT_3D('',#8593,#6789,#6790);
#5541=AXIS2_PLACEMENT_3D('',#8594,#6791,#6792);
#5542=AXIS2_PLACEMENT_3D('',#8595,#6793,#6794);
#5543=AXIS2_PLACEMENT_3D('',#8596,#6795,#6796);
#5544=AXIS2_PLACEMENT_3D('',#8598,#6797,#6798);
#5545=AXIS2_PLACEMENT_3D('',#8601,#6800,#6801);
#5546=AXIS2_PLACEMENT_3D('',#8602,#6802,#6803);
#5547=AXIS2_PLACEMENT_3D('',#8603,#6804,#6805);
#5548=AXIS2_PLACEMENT_3D('',#8605,#6806,#6807);
#5549=AXIS2_PLACEMENT_3D('',#8608,#6809,#6810);
#5550=AXIS2_PLACEMENT_3D('',#8609,#6811,#6812);
#5551=AXIS2_PLACEMENT_3D('',#8610,#6813,#6814);
#5552=AXIS2_PLACEMENT_3D('',#8612,#6815,#6816);
#5553=AXIS2_PLACEMENT_3D('',#8613,#6817,#6818);
#5554=AXIS2_PLACEMENT_3D('',#8616,#6820,#6821);
#5555=AXIS2_PLACEMENT_3D('',#8617,#6822,#6823);
#5556=AXIS2_PLACEMENT_3D('',#8618,#6824,#6825);
#5557=AXIS2_PLACEMENT_3D('',#8619,#6826,#6827);
#5558=AXIS2_PLACEMENT_3D('',#8621,#6828,#6829);
#5559=AXIS2_PLACEMENT_3D('',#8622,#6830,#6831);
#5560=AXIS2_PLACEMENT_3D('',#8624,#6832,#6833);
#5561=AXIS2_PLACEMENT_3D('',#8626,#6835,#6836);
#5562=AXIS2_PLACEMENT_3D('',#8627,#6837,#6838);
#5563=AXIS2_PLACEMENT_3D('',#8628,#6839,#6840);
#5564=AXIS2_PLACEMENT_3D('',#8630,#6841,#6842);
#5565=AXIS2_PLACEMENT_3D('',#8633,#6844,#6845);
#5566=AXIS2_PLACEMENT_3D('',#8634,#6846,#6847);
#5567=AXIS2_PLACEMENT_3D('',#8635,#6848,#6849);
#5568=AXIS2_PLACEMENT_3D('',#8637,#6850,#6851);
#5569=AXIS2_PLACEMENT_3D('',#8640,#6853,#6854);
#5570=AXIS2_PLACEMENT_3D('',#8641,#6855,#6856);
#5571=AXIS2_PLACEMENT_3D('',#8642,#6857,#6858);
#5572=AXIS2_PLACEMENT_3D('',#8644,#6859,#6860);
#5573=AXIS2_PLACEMENT_3D('',#8645,#6861,#6862);
#5574=AXIS2_PLACEMENT_3D('',#8647,#6863,#6864);
#5575=AXIS2_PLACEMENT_3D('',#8649,#6866,#6867);
#5576=AXIS2_PLACEMENT_3D('',#8650,#6868,#6869);
#5577=AXIS2_PLACEMENT_3D('',#8651,#6870,#6871);
#5578=AXIS2_PLACEMENT_3D('',#8653,#6872,#6873);
#5579=AXIS2_PLACEMENT_3D('',#8655,#6874,#6875);
#5580=AXIS2_PLACEMENT_3D('',#8656,#6876,#6877);
#5581=AXIS2_PLACEMENT_3D('',#8657,#6878,#6879);
#5582=AXIS2_PLACEMENT_3D('',#8659,#6880,#6881);
#5583=AXIS2_PLACEMENT_3D('',#8662,#6883,#6884);
#5584=AXIS2_PLACEMENT_3D('',#8663,#6885,#6886);
#5585=AXIS2_PLACEMENT_3D('',#8666,#6887,#6888);
#5586=AXIS2_PLACEMENT_3D('',#8667,#6889,#6890);
#5587=AXIS2_PLACEMENT_3D('',#8669,#6892,#6893);
#5588=AXIS2_PLACEMENT_3D('',#8672,#6895,#6896);
#5589=AXIS2_PLACEMENT_3D('',#8673,#6897,#6898);
#5590=AXIS2_PLACEMENT_3D('',#8676,#6900,#6901);
#5591=AXIS2_PLACEMENT_3D('',#8677,#6902,#6903);
#5592=AXIS2_PLACEMENT_3D('',#8679,#6904,#6905);
#5593=AXIS2_PLACEMENT_3D('',#8681,#6907,#6908);
#5594=AXIS2_PLACEMENT_3D('',#8682,#6909,#6910);
#5595=AXIS2_PLACEMENT_3D('',#8683,#6911,#6912);
#5596=AXIS2_PLACEMENT_3D('',#8686,#6913,#6914);
#5597=AXIS2_PLACEMENT_3D('',#8687,#6915,#6916);
#5598=AXIS2_PLACEMENT_3D('',#8689,#6917,#6918);
#5599=AXIS2_PLACEMENT_3D('',#8692,#6920,#6921);
#5600=AXIS2_PLACEMENT_3D('',#8693,#6922,#6923);
#5601=AXIS2_PLACEMENT_3D('',#8695,#6924,#6925);
#5602=AXIS2_PLACEMENT_3D('',#8698,#6927,#6928);
#5603=AXIS2_PLACEMENT_3D('',#8699,#6929,#6930);
#5604=AXIS2_PLACEMENT_3D('',#8701,#6931,#6932);
#5605=AXIS2_PLACEMENT_3D('',#8702,#6933,#6934);
#5606=AXIS2_PLACEMENT_3D('',#8703,#6935,#6936);
#5607=AXIS2_PLACEMENT_3D('',#8706,#6938,#6939);
#5608=AXIS2_PLACEMENT_3D('',#8707,#6940,#6941);
#5609=AXIS2_PLACEMENT_3D('',#8710,#6942,#6943);
#5610=AXIS2_PLACEMENT_3D('',#8713,#6945,#6946);
#5611=AXIS2_PLACEMENT_3D('',#8714,#6947,#6948);
#5612=AXIS2_PLACEMENT_3D('',#8715,#6949,#6950);
#5613=AXIS2_PLACEMENT_3D('',#8717,#6952,#6953);
#5614=AXIS2_PLACEMENT_3D('',#8718,#6954,#6955);
#5615=AXIS2_PLACEMENT_3D('',#8719,#6956,#6957);
#5616=AXIS2_PLACEMENT_3D('',#8722,#6958,#6959);
#5617=AXIS2_PLACEMENT_3D('',#8723,#6960,#6961);
#5618=AXIS2_PLACEMENT_3D('',#8726,#6962,#6963);
#5619=AXIS2_PLACEMENT_3D('',#8727,#6964,#6965);
#5620=AXIS2_PLACEMENT_3D('',#8730,#6966,#6967);
#5621=AXIS2_PLACEMENT_3D('',#8731,#6968,#6969);
#5622=AXIS2_PLACEMENT_3D('',#8734,#6970,#6971);
#5623=AXIS2_PLACEMENT_3D('',#8735,#6972,#6973);
#5624=AXIS2_PLACEMENT_3D('',#8738,#6974,#6975);
#5625=AXIS2_PLACEMENT_3D('',#8739,#6976,#6977);
#5626=AXIS2_PLACEMENT_3D('',#8742,#6978,#6979);
#5627=AXIS2_PLACEMENT_3D('',#8743,#6980,#6981);
#5628=AXIS2_PLACEMENT_3D('',#8746,#6982,#6983);
#5629=AXIS2_PLACEMENT_3D('',#8747,#6984,#6985);
#5630=AXIS2_PLACEMENT_3D('',#8749,#6986,#6987);
#5631=AXIS2_PLACEMENT_3D('',#8751,#6988,#6989);
#5632=AXIS2_PLACEMENT_3D('',#8752,#6990,#6991);
#5633=AXIS2_PLACEMENT_3D('',#8753,#6992,#6993);
#5634=AXIS2_PLACEMENT_3D('',#8756,#6994,#6995);
#5635=AXIS2_PLACEMENT_3D('',#8758,#6996,#6997);
#5636=AXIS2_PLACEMENT_3D('',#8760,#6998,#6999);
#5637=AXIS2_PLACEMENT_3D('',#8761,#7000,#7001);
#5638=AXIS2_PLACEMENT_3D('',#8762,#7002,#7003);
#5639=AXIS2_PLACEMENT_3D('',#8763,#7004,#7005);
#5640=AXIS2_PLACEMENT_3D('',#8765,#7006,#7007);
#5641=AXIS2_PLACEMENT_3D('',#8767,#7008,#7009);
#5642=AXIS2_PLACEMENT_3D('',#8768,#7010,#7011);
#5643=AXIS2_PLACEMENT_3D('',#8769,#7012,#7013);
#5644=AXIS2_PLACEMENT_3D('',#8772,#7014,#7015);
#5645=AXIS2_PLACEMENT_3D('',#8774,#7016,#7017);
#5646=AXIS2_PLACEMENT_3D('',#8776,#7018,#7019);
#5647=AXIS2_PLACEMENT_3D('',#8777,#7020,#7021);
#5648=AXIS2_PLACEMENT_3D('',#8778,#7022,#7023);
#5649=AXIS2_PLACEMENT_3D('',#8779,#7024,#7025);
#5650=AXIS2_PLACEMENT_3D('',#8781,#7026,#7027);
#5651=AXIS2_PLACEMENT_3D('',#8783,#7028,#7029);
#5652=AXIS2_PLACEMENT_3D('',#8784,#7030,#7031);
#5653=AXIS2_PLACEMENT_3D('',#8785,#7032,#7033);
#5654=AXIS2_PLACEMENT_3D('',#8788,#7034,#7035);
#5655=AXIS2_PLACEMENT_3D('',#8790,#7036,#7037);
#5656=AXIS2_PLACEMENT_3D('',#8792,#7038,#7039);
#5657=AXIS2_PLACEMENT_3D('',#8793,#7040,#7041);
#5658=AXIS2_PLACEMENT_3D('',#8794,#7042,#7043);
#5659=AXIS2_PLACEMENT_3D('',#8795,#7044,#7045);
#5660=AXIS2_PLACEMENT_3D('',#8797,#7046,#7047);
#5661=AXIS2_PLACEMENT_3D('',#8799,#7048,#7049);
#5662=AXIS2_PLACEMENT_3D('',#8800,#7050,#7051);
#5663=AXIS2_PLACEMENT_3D('',#8801,#7052,#7053);
#5664=AXIS2_PLACEMENT_3D('',#8804,#7054,#7055);
#5665=AXIS2_PLACEMENT_3D('',#8806,#7056,#7057);
#5666=AXIS2_PLACEMENT_3D('',#8808,#7058,#7059);
#5667=AXIS2_PLACEMENT_3D('',#8809,#7060,#7061);
#5668=AXIS2_PLACEMENT_3D('',#8810,#7062,#7063);
#5669=AXIS2_PLACEMENT_3D('',#8811,#7064,#7065);
#5670=AXIS2_PLACEMENT_3D('',#8813,#7066,#7067);
#5671=AXIS2_PLACEMENT_3D('',#8815,#7068,#7069);
#5672=AXIS2_PLACEMENT_3D('',#8816,#7070,#7071);
#5673=AXIS2_PLACEMENT_3D('',#8817,#7072,#7073);
#5674=AXIS2_PLACEMENT_3D('',#8820,#7074,#7075);
#5675=AXIS2_PLACEMENT_3D('',#8822,#7076,#7077);
#5676=AXIS2_PLACEMENT_3D('',#8824,#7078,#7079);
#5677=AXIS2_PLACEMENT_3D('',#8825,#7080,#7081);
#5678=AXIS2_PLACEMENT_3D('',#8826,#7082,#7083);
#5679=AXIS2_PLACEMENT_3D('',#8827,#7084,#7085);
#5680=AXIS2_PLACEMENT_3D('',#8829,#7086,#7087);
#5681=AXIS2_PLACEMENT_3D('',#8831,#7088,#7089);
#5682=AXIS2_PLACEMENT_3D('',#8832,#7090,#7091);
#5683=AXIS2_PLACEMENT_3D('',#8833,#7092,#7093);
#5684=AXIS2_PLACEMENT_3D('',#8836,#7094,#7095);
#5685=AXIS2_PLACEMENT_3D('',#8838,#7096,#7097);
#5686=AXIS2_PLACEMENT_3D('',#8840,#7098,#7099);
#5687=AXIS2_PLACEMENT_3D('',#8841,#7100,#7101);
#5688=AXIS2_PLACEMENT_3D('',#8842,#7102,#7103);
#5689=AXIS2_PLACEMENT_3D('',#8843,#7104,#7105);
#5690=AXIS2_PLACEMENT_3D('',#8845,#7106,#7107);
#5691=AXIS2_PLACEMENT_3D('',#8847,#7108,#7109);
#5692=AXIS2_PLACEMENT_3D('',#8848,#7110,#7111);
#5693=AXIS2_PLACEMENT_3D('',#8849,#7112,#7113);
#5694=AXIS2_PLACEMENT_3D('',#8852,#7114,#7115);
#5695=AXIS2_PLACEMENT_3D('',#8854,#7116,#7117);
#5696=AXIS2_PLACEMENT_3D('',#8856,#7118,#7119);
#5697=AXIS2_PLACEMENT_3D('',#8857,#7120,#7121);
#5698=AXIS2_PLACEMENT_3D('',#8858,#7122,#7123);
#5699=AXIS2_PLACEMENT_3D('',#8859,#7124,#7125);
#5700=AXIS2_PLACEMENT_3D('',#8861,#7126,#7127);
#5701=AXIS2_PLACEMENT_3D('',#8863,#7128,#7129);
#5702=AXIS2_PLACEMENT_3D('',#8864,#7130,#7131);
#5703=AXIS2_PLACEMENT_3D('',#8865,#7132,#7133);
#5704=AXIS2_PLACEMENT_3D('',#8868,#7134,#7135);
#5705=AXIS2_PLACEMENT_3D('',#8870,#7136,#7137);
#5706=AXIS2_PLACEMENT_3D('',#8872,#7138,#7139);
#5707=AXIS2_PLACEMENT_3D('',#8873,#7140,#7141);
#5708=AXIS2_PLACEMENT_3D('',#8874,#7142,#7143);
#5709=AXIS2_PLACEMENT_3D('',#8875,#7144,#7145);
#5710=AXIS2_PLACEMENT_3D('',#8877,#7146,#7147);
#5711=AXIS2_PLACEMENT_3D('',#8880,#7149,#7150);
#5712=AXIS2_PLACEMENT_3D('',#8881,#7151,#7152);
#5713=AXIS2_PLACEMENT_3D('',#8883,#7153,#7154);
#5714=AXIS2_PLACEMENT_3D('',#8886,#7156,#7157);
#5715=AXIS2_PLACEMENT_3D('',#8887,#7158,#7159);
#5716=AXIS2_PLACEMENT_3D('',#8888,#7160,#7161);
#5717=AXIS2_PLACEMENT_3D('',#8889,#7162,#7163);
#5718=AXIS2_PLACEMENT_3D('',#8891,#7164,#7165);
#5719=AXIS2_PLACEMENT_3D('',#8893,#7166,#7167);
#5720=AXIS2_PLACEMENT_3D('',#8895,#7168,#7169);
#5721=AXIS2_PLACEMENT_3D('',#8896,#7170,#7171);
#5722=AXIS2_PLACEMENT_3D('',#8897,#7172,#7173);
#5723=AXIS2_PLACEMENT_3D('',#8900,#7174,#7175);
#5724=AXIS2_PLACEMENT_3D('',#8901,#7176,#7177);
#5725=AXIS2_PLACEMENT_3D('',#8903,#7178,#7179);
#5726=AXIS2_PLACEMENT_3D('',#8904,#7180,#7181);
#5727=AXIS2_PLACEMENT_3D('',#8905,#7182,#7183);
#5728=AXIS2_PLACEMENT_3D('',#8909,#7185,#7186);
#5729=AXIS2_PLACEMENT_3D('',#8910,#7187,#7188);
#5730=AXIS2_PLACEMENT_3D('',#8911,#7189,#7190);
#5731=AXIS2_PLACEMENT_3D('',#8913,#7191,#7192);
#5732=AXIS2_PLACEMENT_3D('',#8915,#7194,#7195);
#5733=AXIS2_PLACEMENT_3D('',#8917,#7196,#7197);
#5734=AXIS2_PLACEMENT_3D('',#8920,#7199,#7200);
#5735=AXIS2_PLACEMENT_3D('',#8921,#7201,#7202);
#5736=AXIS2_PLACEMENT_3D('',#8923,#7204,#7205);
#5737=AXIS2_PLACEMENT_3D('',#8924,#7206,#7207);
#5738=AXIS2_PLACEMENT_3D('',#8925,#7208,#7209);
#5739=AXIS2_PLACEMENT_3D('',#8927,#7210,#7211);
#5740=AXIS2_PLACEMENT_3D('',#8929,#7212,#7213);
#5741=AXIS2_PLACEMENT_3D('',#8930,#7214,#7215);
#5742=AXIS2_PLACEMENT_3D('',#8931,#7216,#7217);
#5743=AXIS2_PLACEMENT_3D('',#8933,#7218,#7219);
#5744=AXIS2_PLACEMENT_3D('',#8935,#7220,#7221);
#5745=AXIS2_PLACEMENT_3D('',#8936,#7222,#7223);
#5746=AXIS2_PLACEMENT_3D('',#8937,#7224,#7225);
#5747=AXIS2_PLACEMENT_3D('',#8941,#7227,#7228);
#5748=AXIS2_PLACEMENT_3D('',#8942,#7229,#7230);
#5749=AXIS2_PLACEMENT_3D('',#8943,#7231,#7232);
#5750=AXIS2_PLACEMENT_3D('',#8945,#7233,#7234);
#5751=AXIS2_PLACEMENT_3D('',#8947,#7236,#7237);
#5752=AXIS2_PLACEMENT_3D('',#8949,#7238,#7239);
#5753=AXIS2_PLACEMENT_3D('',#8952,#7241,#7242);
#5754=AXIS2_PLACEMENT_3D('',#8953,#7243,#7244);
#5755=AXIS2_PLACEMENT_3D('',#8955,#7246,#7247);
#5756=AXIS2_PLACEMENT_3D('',#8956,#7248,#7249);
#5757=AXIS2_PLACEMENT_3D('',#8957,#7250,#7251);
#5758=AXIS2_PLACEMENT_3D('',#8958,#7252,#7253);
#5759=AXIS2_PLACEMENT_3D('',#8960,#7254,#7255);
#5760=AXIS2_PLACEMENT_3D('',#9000,#7257,#7258);
#5761=AXIS2_PLACEMENT_3D('',#9041,#7260,#7261);
#5762=AXIS2_PLACEMENT_3D('',#9042,#7262,#7263);
#5763=AXIS2_PLACEMENT_3D('',#9044,#7264,#7265);
#5764=AXIS2_PLACEMENT_3D('',#9084,#7267,#7268);
#5765=AXIS2_PLACEMENT_3D('',#9125,#7270,#7271);
#5766=AXIS2_PLACEMENT_3D('',#9126,#7272,#7273);
#5767=AXIS2_PLACEMENT_3D('',#9128,#7274,#7275);
#5768=AXIS2_PLACEMENT_3D('',#9168,#7277,#7278);
#5769=AXIS2_PLACEMENT_3D('',#9209,#7280,#7281);
#5770=AXIS2_PLACEMENT_3D('',#9210,#7282,#7283);
#5771=AXIS2_PLACEMENT_3D('',#9212,#7284,#7285);
#5772=AXIS2_PLACEMENT_3D('',#9252,#7287,#7288);
#5773=AXIS2_PLACEMENT_3D('',#9293,#7290,#7291);
#5774=AXIS2_PLACEMENT_3D('',#9294,#7292,#7293);
#5775=AXIS2_PLACEMENT_3D('',#9303,#7298,#7299);
#5776=AXIS2_PLACEMENT_3D('',#9309,#7303,#7304);
#5777=AXIS2_PLACEMENT_3D('',#9315,#7308,#7309);
#5778=AXIS2_PLACEMENT_3D('',#9321,#7313,#7314);
#5779=AXIS2_PLACEMENT_3D('',#9327,#7318,#7319);
#5780=AXIS2_PLACEMENT_3D('',#9366,#7339,#7340);
#5781=AXIS2_PLACEMENT_3D('',#9368,#7341,#7342);
#5782=AXIS2_PLACEMENT_3D('',#9370,#7343,#7344);
#5783=AXIS2_PLACEMENT_3D('',#9371,#7345,#7346);
#5784=AXIS2_PLACEMENT_3D('',#9377,#7350,#7351);
#5785=AXIS2_PLACEMENT_3D('',#9381,#7354,#7355);
#5786=AXIS2_PLACEMENT_3D('',#9383,#7357,#7358);
#5787=AXIS2_PLACEMENT_3D('',#9416,#7375,#7376);
#5788=AXIS2_PLACEMENT_3D('',#9418,#7377,#7378);
#5789=AXIS2_PLACEMENT_3D('',#9420,#7379,#7380);
#5790=AXIS2_PLACEMENT_3D('',#9421,#7381,#7382);
#5791=AXIS2_PLACEMENT_3D('',#9423,#7384,#7385);
#5792=AXIS2_PLACEMENT_3D('',#9426,#7388,#7389);
#5793=AXIS2_PLACEMENT_3D('',#9428,#7391,#7392);
#5794=AXIS2_PLACEMENT_3D('',#9430,#7394,#7395);
#5795=AXIS2_PLACEMENT_3D('',#9432,#7397,#7398);
#5796=AXIS2_PLACEMENT_3D('',#9434,#7400,#7401);
#5797=AXIS2_PLACEMENT_3D('',#9437,#7404,#7405);
#5798=AXIS2_PLACEMENT_3D('',#9439,#7407,#7408);
#5799=AXIS2_PLACEMENT_3D('',#9440,#7409,#7410);
#5800=AXIS2_PLACEMENT_3D('',#9442,#7412,#7413);
#5801=AXIS2_PLACEMENT_3D('',#9444,#7415,#7416);
#5802=AXIS2_PLACEMENT_3D('',#9446,#7418,#7419);
#5803=AXIS2_PLACEMENT_3D('',#9448,#7421,#7422);
#5804=AXIS2_PLACEMENT_3D('',#9450,#7424,#7425);
#5805=AXIS2_PLACEMENT_3D('',#9452,#7427,#7428);
#5806=AXIS2_PLACEMENT_3D('',#9453,#7429,#7430);
#5807=AXIS2_PLACEMENT_3D('',#9455,#7432,#7433);
#5808=AXIS2_PLACEMENT_3D('',#9457,#7435,#7436);
#5809=AXIS2_PLACEMENT_3D('',#9458,#7437,#7438);
#5810=AXIS2_PLACEMENT_3D('',#9459,#7439,#7440);
#5811=AXIS2_PLACEMENT_3D('',#9460,#7441,#7442);
#5812=AXIS2_PLACEMENT_3D('',#9461,#7443,#7444);
#5813=AXIS2_PLACEMENT_3D('',#9462,#7445,#7446);
#5814=AXIS2_PLACEMENT_3D('',#9463,#7447,#7448);
#5815=AXIS2_PLACEMENT_3D('',#9464,#7449,#7450);
#5816=AXIS2_PLACEMENT_3D('',#9465,#7451,#7452);
#5817=AXIS2_PLACEMENT_3D('',#9466,#7453,#7454);
#5818=AXIS2_PLACEMENT_3D('',#9467,#7455,#7456);
#5819=AXIS2_PLACEMENT_3D('',#9468,#7457,#7458);
#5820=AXIS2_PLACEMENT_3D('',#9469,#7459,#7460);
#5821=AXIS2_PLACEMENT_3D('',#9470,#7461,#7462);
#5822=AXIS2_PLACEMENT_3D('',#9471,#7463,#7464);
#5823=AXIS2_PLACEMENT_3D('',#9472,#7465,#7466);
#5824=AXIS2_PLACEMENT_3D('',#9473,#7467,#7468);
#5825=AXIS2_PLACEMENT_3D('',#9474,#7469,#7470);
#5826=DIRECTION('axis',(0.,0.,1.));
#5827=DIRECTION('refdir',(1.,0.,0.));
#5828=DIRECTION('axis',(0.,0.,1.));
#5829=DIRECTION('refdir',(1.,0.,0.));
#5830=DIRECTION('center_axis',(-1.,0.,0.));
#5831=DIRECTION('ref_axis',(0.,1.,0.));
#5832=DIRECTION('center_axis',(-1.,0.,0.));
#5833=DIRECTION('ref_axis',(0.,1.,0.));
#5834=DIRECTION('',(-1.,0.,0.));
#5835=DIRECTION('center_axis',(-1.,0.,0.));
#5836=DIRECTION('ref_axis',(0.,1.,0.));
#5837=DIRECTION('center_axis',(1.,0.,0.));
#5838=DIRECTION('ref_axis',(0.,1.,0.));
#5839=DIRECTION('center_axis',(1.,0.,0.));
#5840=DIRECTION('ref_axis',(0.,1.,0.));
#5841=DIRECTION('center_axis',(0.,0.,-1.));
#5842=DIRECTION('ref_axis',(1.,0.,0.));
#5843=DIRECTION('center_axis',(0.,0.,-1.));
#5844=DIRECTION('ref_axis',(1.,0.,0.));
#5845=DIRECTION('',(0.,0.,-1.));
#5846=DIRECTION('center_axis',(0.,0.,-1.));
#5847=DIRECTION('ref_axis',(1.,0.,0.));
#5848=DIRECTION('center_axis',(0.,0.,1.));
#5849=DIRECTION('ref_axis',(1.,0.,0.));
#5850=DIRECTION('center_axis',(0.,0.,-1.));
#5851=DIRECTION('ref_axis',(1.,0.,0.));
#5852=DIRECTION('center_axis',(0.,0.,-1.));
#5853=DIRECTION('ref_axis',(1.,0.,0.));
#5854=DIRECTION('',(0.,0.,-1.));
#5855=DIRECTION('center_axis',(0.,0.,-1.));
#5856=DIRECTION('ref_axis',(1.,0.,0.));
#5857=DIRECTION('center_axis',(0.,0.,1.));
#5858=DIRECTION('ref_axis',(1.,0.,0.));
#5859=DIRECTION('center_axis',(0.,1.,0.));
#5860=DIRECTION('ref_axis',(1.,0.,0.));
#5861=DIRECTION('center_axis',(0.,1.,0.));
#5862=DIRECTION('ref_axis',(1.,0.,0.));
#5863=DIRECTION('',(0.,1.,0.));
#5864=DIRECTION('center_axis',(0.,1.,0.));
#5865=DIRECTION('ref_axis',(1.,0.,0.));
#5866=DIRECTION('center_axis',(0.,-1.,0.));
#5867=DIRECTION('ref_axis',(1.,0.,0.));
#5868=DIRECTION('center_axis',(0.,-1.,0.));
#5869=DIRECTION('ref_axis',(1.,0.,0.));
#5870=DIRECTION('center_axis',(0.,1.,0.));
#5871=DIRECTION('ref_axis',(1.,0.,0.));
#5872=DIRECTION('',(0.,1.,0.));
#5873=DIRECTION('center_axis',(0.,-1.,0.));
#5874=DIRECTION('ref_axis',(1.,0.,0.));
#5875=DIRECTION('center_axis',(0.,1.,0.));
#5876=DIRECTION('ref_axis',(1.,0.,0.));
#5877=DIRECTION('center_axis',(0.,1.,0.));
#5878=DIRECTION('ref_axis',(1.,0.,0.));
#5879=DIRECTION('',(0.,1.,0.));
#5880=DIRECTION('center_axis',(0.,1.,0.));
#5881=DIRECTION('ref_axis',(1.,0.,0.));
#5882=DIRECTION('center_axis',(0.,-1.,0.));
#5883=DIRECTION('ref_axis',(1.,0.,0.));
#5884=DIRECTION('center_axis',(-1.,0.,0.));
#5885=DIRECTION('ref_axis',(0.,1.,0.));
#5886=DIRECTION('',(-1.,0.,0.));
#5887=DIRECTION('center_axis',(1.,0.,0.));
#5888=DIRECTION('ref_axis',(0.,1.,0.));
#5889=DIRECTION('center_axis',(1.,0.,0.));
#5890=DIRECTION('ref_axis',(0.,-6.12323399573677E-17,-1.));
#5891=DIRECTION('',(-1.,0.,0.));
#5892=DIRECTION('center_axis',(-1.,0.,0.));
#5893=DIRECTION('ref_axis',(0.,-1.,0.));
#5894=DIRECTION('',(1.,0.,0.));
#5895=DIRECTION('center_axis',(1.,0.,0.));
#5896=DIRECTION('ref_axis',(0.,-1.,0.));
#5897=DIRECTION('center_axis',(-1.,0.,0.));
#5898=DIRECTION('ref_axis',(0.,-1.,0.));
#5899=DIRECTION('',(0.,0.,1.));
#5900=DIRECTION('',(0.,-1.,0.));
#5901=DIRECTION('',(0.,0.,1.));
#5902=DIRECTION('',(0.,1.,0.));
#5903=DIRECTION('',(0.,0.,-1.));
#5904=DIRECTION('',(0.,-1.,0.));
#5905=DIRECTION('',(0.,0.,-1.));
#5906=DIRECTION('center_axis',(0.,1.,0.));
#5907=DIRECTION('ref_axis',(1.,0.,0.));
#5908=DIRECTION('',(0.,0.,-1.));
#5909=DIRECTION('',(-1.,0.,0.));
#5910=DIRECTION('',(0.,0.,-1.));
#5911=DIRECTION('center_axis',(0.,1.,0.));
#5912=DIRECTION('ref_axis',(0.70710678118654,0.,0.707106781186555));
#5913=DIRECTION('',(1.,0.,0.));
#5914=DIRECTION('center_axis',(0.,1.,0.));
#5915=DIRECTION('ref_axis',(-0.70710678118654,0.,0.707106781186555));
#5916=DIRECTION('center_axis',(1.,0.,0.));
#5917=DIRECTION('ref_axis',(0.,1.,0.));
#5918=DIRECTION('',(0.,0.,1.));
#5919=DIRECTION('center_axis',(-1.,0.,0.));
#5920=DIRECTION('ref_axis',(0.,1.,0.));
#5921=DIRECTION('center_axis',(0.,-1.,0.));
#5922=DIRECTION('ref_axis',(-1.,0.,0.));
#5923=DIRECTION('center_axis',(0.,-1.,0.));
#5924=DIRECTION('ref_axis',(-0.70710678118654,0.,0.707106781186555));
#5925=DIRECTION('',(-1.,0.,0.));
#5926=DIRECTION('center_axis',(0.,-1.,0.));
#5927=DIRECTION('ref_axis',(0.70710678118654,0.,0.707106781186555));
#5928=DIRECTION('',(0.,0.,1.));
#5929=DIRECTION('',(1.,0.,0.));
#5930=DIRECTION('center_axis',(0.,-1.,0.));
#5931=DIRECTION('ref_axis',(-0.70710678118654,0.,0.707106781186555));
#5932=DIRECTION('',(0.,1.,0.));
#5933=DIRECTION('center_axis',(0.,1.,0.));
#5934=DIRECTION('ref_axis',(0.,0.,1.));
#5935=DIRECTION('center_axis',(0.,0.,1.));
#5936=DIRECTION('ref_axis',(1.,0.,0.));
#5937=DIRECTION('',(0.,-1.,0.));
#5938=DIRECTION('',(1.,0.,0.));
#5939=DIRECTION('center_axis',(0.,1.,0.));
#5940=DIRECTION('ref_axis',(0.70710678118654,0.,0.707106781186555));
#5941=DIRECTION('',(0.,1.,0.));
#5942=DIRECTION('center_axis',(0.,1.,0.));
#5943=DIRECTION('ref_axis',(1.,0.,0.));
#5944=DIRECTION('center_axis',(0.,1.,0.));
#5945=DIRECTION('ref_axis',(0.70710678118654,0.,0.707106781186555));
#5946=DIRECTION('',(0.,-1.,0.));
#5947=DIRECTION('center_axis',(0.,-1.,0.));
#5948=DIRECTION('ref_axis',(0.,0.,1.));
#5949=DIRECTION('',(0.,1.,0.));
#5950=DIRECTION('center_axis',(-0.40824829046386,-0.816496580927727,0.408248290463864));
#5951=DIRECTION('ref_axis',(0.577350269189625,-0.577350269189625,-0.577350269189628));
#5952=DIRECTION('center_axis',(0.,-1.,0.));
#5953=DIRECTION('ref_axis',(1.,0.,0.));
#5954=DIRECTION('center_axis',(0.,0.,-1.));
#5955=DIRECTION('ref_axis',(0.,-1.,0.));
#5956=DIRECTION('center_axis',(1.,0.,0.));
#5957=DIRECTION('ref_axis',(0.,0.,-1.));
#5958=DIRECTION('center_axis',(-0.40824829046386,-0.816496580927727,-0.408248290463864));
#5959=DIRECTION('ref_axis',(0.577350269189625,-0.577350269189625,0.577350269189628));
#5960=DIRECTION('center_axis',(1.,0.,0.));
#5961=DIRECTION('ref_axis',(0.,-1.,0.));
#5962=DIRECTION('center_axis',(0.,0.,1.));
#5963=DIRECTION('ref_axis',(1.,0.,0.));
#5964=DIRECTION('center_axis',(0.,0.,1.));
#5965=DIRECTION('ref_axis',(0.707106781186541,-0.707106781186554,0.));
#5966=DIRECTION('',(0.,0.,-1.));
#5967=DIRECTION('',(0.,0.,1.));
#5968=DIRECTION('center_axis',(0.40824829046386,-0.816496580927727,0.408248290463864));
#5969=DIRECTION('ref_axis',(-0.577350269189625,-0.577350269189625,-0.577350269189628));
#5970=DIRECTION('center_axis',(-1.,0.,0.));
#5971=DIRECTION('ref_axis',(0.,-1.,0.));
#5972=DIRECTION('center_axis',(0.,0.,-1.));
#5973=DIRECTION('ref_axis',(-1.,0.,0.));
#5974=DIRECTION('center_axis',(0.,-1.,0.));
#5975=DIRECTION('ref_axis',(0.,0.,-1.));
#5976=DIRECTION('center_axis',(0.408248290463862,0.408248290463855,-0.816496580927731));
#5977=DIRECTION('ref_axis',(0.577350269189628,0.577350269189628,0.577350269189621));
#5978=DIRECTION('center_axis',(0.,0.,1.));
#5979=DIRECTION('ref_axis',(0.,1.,0.));
#5980=DIRECTION('center_axis',(1.,1.77635683940026E-14,0.));
#5981=DIRECTION('ref_axis',(0.,0.,1.));
#5982=DIRECTION('center_axis',(0.,0.,1.));
#5983=DIRECTION('ref_axis',(0.707106781186554,0.707106781186541,0.));
#5984=DIRECTION('',(0.,0.,1.));
#5985=DIRECTION('',(0.,0.,-1.));
#5986=DIRECTION('center_axis',(0.,0.707106781186549,0.707106781186546));
#5987=DIRECTION('ref_axis',(0.,0.707106781186546,-0.707106781186549));
#5988=DIRECTION('center_axis',(0.40824829046386,-0.816496580927727,-0.408248290463864));
#5989=DIRECTION('ref_axis',(-0.577350269189625,-0.577350269189625,0.577350269189628));
#5990=DIRECTION('center_axis',(0.,-1.,0.));
#5991=DIRECTION('ref_axis',(-1.,0.,0.));
#5992=DIRECTION('center_axis',(0.,0.,1.));
#5993=DIRECTION('ref_axis',(0.,-1.,0.));
#5994=DIRECTION('center_axis',(-1.,0.,0.));
#5995=DIRECTION('ref_axis',(0.,0.,1.));
#5996=DIRECTION('center_axis',(0.,0.,-1.));
#5997=DIRECTION('ref_axis',(-0.707106781186541,-0.707106781186554,0.));
#5998=DIRECTION('',(0.,0.,1.));
#5999=DIRECTION('center_axis',(1.,0.,0.));
#6000=DIRECTION('ref_axis',(0.,-0.707106781186546,0.707106781186549));
#6001=DIRECTION('',(-1.,0.,0.));
#6002=DIRECTION('',(1.,0.,0.));
#6003=DIRECTION('center_axis',(-0.40824829046386,-0.816496580927727,0.408248290463864));
#6004=DIRECTION('ref_axis',(-0.577350269189625,0.577350269189625,0.577350269189628));
#6005=DIRECTION('center_axis',(-1.,0.,0.));
#6006=DIRECTION('ref_axis',(0.,1.,0.));
#6007=DIRECTION('center_axis',(0.,0.,1.));
#6008=DIRECTION('ref_axis',(-1.,0.,0.));
#6009=DIRECTION('center_axis',(0.,0.,1.));
#6010=DIRECTION('ref_axis',(-0.707106781186541,0.707106781186554,0.));
#6011=DIRECTION('',(0.,0.,-1.));
#6012=DIRECTION('center_axis',(0.,0.707106781186549,0.707106781186546));
#6013=DIRECTION('ref_axis',(0.,0.707106781186546,-0.707106781186549));
#6014=DIRECTION('center_axis',(0.,-1.,0.));
#6015=DIRECTION('ref_axis',(-0.70710678118654,0.,0.707106781186555));
#6016=DIRECTION('',(0.,1.,0.));
#6017=DIRECTION('center_axis',(-1.,0.,0.));
#6018=DIRECTION('ref_axis',(0.,0.707106781186546,0.707106781186549));
#6019=DIRECTION('',(-1.,0.,0.));
#6020=DIRECTION('center_axis',(0.,1.,0.));
#6021=DIRECTION('ref_axis',(-0.70710678118654,0.,-0.707106781186555));
#6022=DIRECTION('',(0.,-1.,0.));
#6023=DIRECTION('center_axis',(-1.,0.,0.));
#6024=DIRECTION('ref_axis',(0.,-0.707106781186546,-0.707106781186549));
#6025=DIRECTION('',(1.,0.,0.));
#6026=DIRECTION('',(-1.,0.,0.));
#6027=DIRECTION('center_axis',(0.,-1.,0.));
#6028=DIRECTION('ref_axis',(0.70710678118654,0.,-0.707106781186555));
#6029=DIRECTION('',(0.,-1.,0.));
#6030=DIRECTION('',(0.,1.,0.));
#6031=DIRECTION('center_axis',(0.,0.,-1.));
#6032=DIRECTION('ref_axis',(-1.,0.,0.));
#6033=DIRECTION('',(1.,0.,0.));
#6034=DIRECTION('center_axis',(1.,0.,0.));
#6035=DIRECTION('ref_axis',(0.,1.,0.));
#6036=DIRECTION('center_axis',(-1.,0.,0.));
#6037=DIRECTION('ref_axis',(0.,1.,0.));
#6038=DIRECTION('center_axis',(-1.,0.,0.));
#6039=DIRECTION('ref_axis',(0.,1.,0.));
#6040=DIRECTION('center_axis',(0.,-1.,0.));
#6041=DIRECTION('ref_axis',(1.,0.,0.));
#6042=DIRECTION('center_axis',(0.,0.,1.));
#6043=DIRECTION('ref_axis',(1.,0.,0.));
#6044=DIRECTION('center_axis',(1.,0.,0.));
#6045=DIRECTION('ref_axis',(0.,-1.83697019872103E-16,-1.));
#6046=DIRECTION('center_axis',(1.,0.,0.));
#6047=DIRECTION('ref_axis',(0.,1.,0.));
#6048=DIRECTION('center_axis',(-1.,0.,0.));
#6049=DIRECTION('ref_axis',(0.,1.,0.));
#6050=DIRECTION('center_axis',(1.,0.,0.));
#6051=DIRECTION('ref_axis',(0.,1.,0.));
#6052=DIRECTION('',(1.,0.,0.));
#6053=DIRECTION('center_axis',(0.,1.,0.));
#6054=DIRECTION('ref_axis',(-1.,0.,0.));
#6055=DIRECTION('axis',(0.,0.,1.));
#6056=DIRECTION('refdir',(1.,0.,0.));
#6057=DIRECTION('center_axis',(-1.,0.,0.));
#6058=DIRECTION('ref_axis',(0.,1.,0.));
#6059=DIRECTION('center_axis',(1.,0.,0.));
#6060=DIRECTION('ref_axis',(0.,1.,0.));
#6061=DIRECTION('',(-1.,0.,0.));
#6062=DIRECTION('center_axis',(1.,0.,0.));
#6063=DIRECTION('ref_axis',(0.,1.,0.));
#6064=DIRECTION('center_axis',(1.,0.,0.));
#6065=DIRECTION('ref_axis',(0.,1.,0.));
#6066=DIRECTION('center_axis',(-1.,0.,0.));
#6067=DIRECTION('ref_axis',(0.,1.,0.));
#6068=DIRECTION('center_axis',(0.,0.,-1.));
#6069=DIRECTION('ref_axis',(1.,0.,0.));
#6070=DIRECTION('center_axis',(0.,0.,-1.));
#6071=DIRECTION('ref_axis',(1.,0.,0.));
#6072=DIRECTION('',(0.,0.,-1.));
#6073=DIRECTION('center_axis',(0.,0.,-1.));
#6074=DIRECTION('ref_axis',(1.,0.,0.));
#6075=DIRECTION('center_axis',(0.,0.,1.));
#6076=DIRECTION('ref_axis',(1.,0.,0.));
#6077=DIRECTION('center_axis',(0.,0.,-1.));
#6078=DIRECTION('ref_axis',(1.,0.,0.));
#6079=DIRECTION('center_axis',(0.,0.,-1.));
#6080=DIRECTION('ref_axis',(1.,0.,0.));
#6081=DIRECTION('',(0.,0.,-1.));
#6082=DIRECTION('center_axis',(0.,0.,-1.));
#6083=DIRECTION('ref_axis',(1.,0.,0.));
#6084=DIRECTION('center_axis',(0.,0.,1.));
#6085=DIRECTION('ref_axis',(1.,0.,0.));
#6086=DIRECTION('center_axis',(-1.,0.,0.));
#6087=DIRECTION('ref_axis',(0.,1.,0.));
#6088=DIRECTION('center_axis',(-1.,0.,0.));
#6089=DIRECTION('ref_axis',(0.,1.,0.));
#6090=DIRECTION('',(-1.,0.,0.));
#6091=DIRECTION('center_axis',(-1.,0.,0.));
#6092=DIRECTION('ref_axis',(0.,1.,0.));
#6093=DIRECTION('center_axis',(1.,0.,0.));
#6094=DIRECTION('ref_axis',(0.,1.,0.));
#6095=DIRECTION('center_axis',(1.,0.,0.));
#6096=DIRECTION('ref_axis',(0.,1.,0.));
#6097=DIRECTION('center_axis',(-1.,0.,0.));
#6098=DIRECTION('ref_axis',(0.,1.,0.));
#6099=DIRECTION('center_axis',(-1.,0.,0.));
#6100=DIRECTION('ref_axis',(0.,1.,0.));
#6101=DIRECTION('',(-1.,0.,0.));
#6102=DIRECTION('center_axis',(-1.,0.,0.));
#6103=DIRECTION('ref_axis',(0.,1.,0.));
#6104=DIRECTION('center_axis',(1.,0.,0.));
#6105=DIRECTION('ref_axis',(0.,1.,0.));
#6106=DIRECTION('center_axis',(1.,0.,0.));
#6107=DIRECTION('ref_axis',(0.,1.,0.));
#6108=DIRECTION('center_axis',(-1.,0.,0.));
#6109=DIRECTION('ref_axis',(0.,1.,0.));
#6110=DIRECTION('',(-1.,0.,0.));
#6111=DIRECTION('center_axis',(-1.,0.,0.));
#6112=DIRECTION('ref_axis',(0.,1.,0.));
#6113=DIRECTION('',(-1.,0.,0.));
#6114=DIRECTION('center_axis',(1.,0.,0.));
#6115=DIRECTION('ref_axis',(0.,1.,0.));
#6116=DIRECTION('center_axis',(-0.40824829046386,-0.816496580927727,-0.408248290463864));
#6117=DIRECTION('ref_axis',(-0.577350269189625,0.577350269189625,-0.577350269189628));
#6118=DIRECTION('center_axis',(0.,1.,0.));
#6119=DIRECTION('ref_axis',(-1.,0.,0.));
#6120=DIRECTION('center_axis',(0.,0.,-1.));
#6121=DIRECTION('ref_axis',(0.,1.,0.));
#6122=DIRECTION('center_axis',(-1.,0.,0.));
#6123=DIRECTION('ref_axis',(0.,0.,-1.));
#6124=DIRECTION('center_axis',(0.408248290463869,0.408248290463855,-0.816496580927727));
#6125=DIRECTION('ref_axis',(-0.577350269189633,-0.577350269189619,-0.577350269189626));
#6126=DIRECTION('center_axis',(-1.,0.,1.77635683940025E-14));
#6127=DIRECTION('ref_axis',(0.,-1.,0.));
#6128=DIRECTION('center_axis',(0.,0.,-1.));
#6129=DIRECTION('ref_axis',(-1.,0.,0.));
#6130=DIRECTION('center_axis',(0.,-1.,0.));
#6131=DIRECTION('ref_axis',(0.,0.,-1.));
#6132=DIRECTION('center_axis',(-0.408248290463856,-0.408248290463856,-0.816496580927733));
#6133=DIRECTION('ref_axis',(0.577350269189645,0.577350269189616,-0.577350269189616));
#6134=DIRECTION('center_axis',(1.,0.,1.77635683940025E-14));
#6135=DIRECTION('ref_axis',(0.,1.,0.));
#6136=DIRECTION('center_axis',(0.,0.,-1.));
#6137=DIRECTION('ref_axis',(1.,0.,0.));
#6138=DIRECTION('center_axis',(0.,1.,0.));
#6139=DIRECTION('ref_axis',(0.,0.,-1.));
#6140=DIRECTION('center_axis',(-0.40824829046386,-0.816496580927727,0.408248290463864));
#6141=DIRECTION('ref_axis',(-0.577350269189625,0.577350269189625,0.577350269189628));
#6142=DIRECTION('center_axis',(-1.,0.,0.));
#6143=DIRECTION('ref_axis',(0.,1.,0.));
#6144=DIRECTION('center_axis',(0.,0.,1.));
#6145=DIRECTION('ref_axis',(-1.,0.,0.));
#6146=DIRECTION('center_axis',(0.,1.,0.));
#6147=DIRECTION('ref_axis',(0.,0.,1.));
#6148=DIRECTION('center_axis',(0.,0.,1.));
#6149=DIRECTION('ref_axis',(-0.707106781186541,0.707106781186554,0.));
#6150=DIRECTION('',(0.,0.,-1.));
#6151=DIRECTION('',(0.,0.,1.));
#6152=DIRECTION('center_axis',(-0.408248290463862,0.408248290463855,-0.816496580927731));
#6153=DIRECTION('ref_axis',(0.577350269189628,-0.577350269189628,-0.577350269189621));
#6154=DIRECTION('center_axis',(0.,-1.,0.));
#6155=DIRECTION('ref_axis',(1.,0.,0.));
#6156=DIRECTION('center_axis',(0.,0.,-1.));
#6157=DIRECTION('ref_axis',(0.,-1.,0.));
#6158=DIRECTION('center_axis',(1.,-1.77635683940026E-14,0.));
#6159=DIRECTION('ref_axis',(0.,0.,-1.));
#6160=DIRECTION('center_axis',(-0.408248290463862,-0.408248290463855,-0.816496580927731));
#6161=DIRECTION('ref_axis',(-0.57735026918964,-0.577350269189619,0.577350269189619));
#6162=DIRECTION('center_axis',(0.,-1.,0.));
#6163=DIRECTION('ref_axis',(-1.,0.,0.));
#6164=DIRECTION('center_axis',(0.,0.,1.));
#6165=DIRECTION('ref_axis',(0.,-1.,0.));
#6166=DIRECTION('center_axis',(-1.,-1.77635683940026E-14,0.));
#6167=DIRECTION('ref_axis',(0.,0.,1.));
#6168=DIRECTION('center_axis',(0.,0.,1.));
#6169=DIRECTION('ref_axis',(-0.707106781186554,-0.707106781186541,0.));
#6170=DIRECTION('',(0.,0.,-1.));
#6171=DIRECTION('',(0.,0.,1.));
#6172=DIRECTION('center_axis',(0.408248290463862,0.408248290463855,-0.816496580927731));
#6173=DIRECTION('ref_axis',(0.577350269189628,0.577350269189628,0.577350269189621));
#6174=DIRECTION('center_axis',(0.,1.,0.));
#6175=DIRECTION('ref_axis',(1.,0.,0.));
#6176=DIRECTION('center_axis',(0.,0.,1.));
#6177=DIRECTION('ref_axis',(0.,1.,0.));
#6178=DIRECTION('center_axis',(1.,1.77635683940026E-14,0.));
#6179=DIRECTION('ref_axis',(0.,0.,1.));
#6180=DIRECTION('center_axis',(0.,0.,1.));
#6181=DIRECTION('ref_axis',(0.707106781186554,0.707106781186541,0.));
#6182=DIRECTION('',(0.,0.,-1.));
#6183=DIRECTION('',(0.,0.,1.));
#6184=DIRECTION('center_axis',(-1.,0.,0.));
#6185=DIRECTION('ref_axis',(0.,0.707106781186546,0.707106781186549));
#6186=DIRECTION('',(1.,0.,0.));
#6187=DIRECTION('',(-1.,0.,0.));
#6188=DIRECTION('center_axis',(0.408248290463856,-0.408248290463856,-0.816496580927733));
#6189=DIRECTION('ref_axis',(0.577350269189645,-0.577350269189616,0.577350269189616));
#6190=DIRECTION('center_axis',(1.,0.,-1.77635683940025E-14));
#6191=DIRECTION('ref_axis',(0.,-1.,0.));
#6192=DIRECTION('center_axis',(0.,0.,1.));
#6193=DIRECTION('ref_axis',(1.,0.,0.));
#6194=DIRECTION('center_axis',(0.,-1.,0.));
#6195=DIRECTION('ref_axis',(0.,0.,1.));
#6196=DIRECTION('center_axis',(0.,0.,-1.));
#6197=DIRECTION('ref_axis',(0.707106781186554,-0.707106781186541,0.));
#6198=DIRECTION('',(0.,0.,1.));
#6199=DIRECTION('',(0.,0.,-1.));
#6200=DIRECTION('center_axis',(0.,1.,0.));
#6201=DIRECTION('ref_axis',(0.70710678118654,0.,0.707106781186555));
#6202=DIRECTION('',(0.,-1.,0.));
#6203=DIRECTION('',(0.,1.,0.));
#6204=DIRECTION('center_axis',(1.,0.,0.));
#6205=DIRECTION('ref_axis',(0.,-0.707106781186546,0.707106781186549));
#6206=DIRECTION('',(-1.,0.,0.));
#6207=DIRECTION('',(1.,0.,0.));
#6208=DIRECTION('center_axis',(0.,-1.,0.));
#6209=DIRECTION('ref_axis',(-0.70710678118654,0.,0.707106781186555));
#6210=DIRECTION('',(0.,1.,0.));
#6211=DIRECTION('',(0.,-1.,0.));
#6212=DIRECTION('center_axis',(-1.,0.,0.));
#6213=DIRECTION('ref_axis',(0.,-0.707106781186546,-0.707106781186549));
#6214=DIRECTION('',(1.,0.,0.));
#6215=DIRECTION('',(-1.,0.,0.));
#6216=DIRECTION('center_axis',(0.,-1.,0.));
#6217=DIRECTION('ref_axis',(0.70710678118654,0.,-0.707106781186555));
#6218=DIRECTION('',(0.,1.,0.));
#6219=DIRECTION('',(0.,-1.,0.));
#6220=DIRECTION('center_axis',(1.,0.,0.));
#6221=DIRECTION('ref_axis',(0.,0.707106781186546,-0.707106781186549));
#6222=DIRECTION('',(-1.,0.,0.));
#6223=DIRECTION('',(1.,0.,0.));
#6224=DIRECTION('center_axis',(0.,1.,0.));
#6225=DIRECTION('ref_axis',(-0.70710678118654,0.,-0.707106781186555));
#6226=DIRECTION('',(0.,-1.,0.));
#6227=DIRECTION('',(0.,1.,0.));
#6228=DIRECTION('center_axis',(-1.,0.,0.));
#6229=DIRECTION('ref_axis',(0.,-1.,0.));
#6230=DIRECTION('center_axis',(1.,0.,0.));
#6231=DIRECTION('ref_axis',(0.,1.,0.));
#6232=DIRECTION('center_axis',(1.,0.,0.));
#6233=DIRECTION('ref_axis',(0.,1.,0.));
#6234=DIRECTION('center_axis',(0.,1.,0.));
#6235=DIRECTION('ref_axis',(-1.,0.,0.));
#6236=DIRECTION('center_axis',(0.,0.,1.));
#6237=DIRECTION('ref_axis',(1.,0.,0.));
#6238=DIRECTION('center_axis',(0.,-1.,0.));
#6239=DIRECTION('ref_axis',(1.,0.,0.));
#6240=DIRECTION('center_axis',(1.,0.,0.));
#6241=DIRECTION('ref_axis',(0.,1.,0.));
#6242=DIRECTION('center_axis',(0.,0.,-1.));
#6243=DIRECTION('ref_axis',(-1.,0.,0.));
#6244=DIRECTION('center_axis',(1.,0.,0.));
#6245=DIRECTION('ref_axis',(0.,1.,0.));
#6246=DIRECTION('',(1.,0.,0.));
#6247=DIRECTION('center_axis',(1.,0.,0.));
#6248=DIRECTION('ref_axis',(0.,1.,0.));
#6249=DIRECTION('center_axis',(1.,0.,0.));
#6250=DIRECTION('ref_axis',(0.,1.,0.));
#6251=DIRECTION('center_axis',(1.,0.,0.));
#6252=DIRECTION('ref_axis',(0.,1.,0.));
#6253=DIRECTION('',(1.,0.,0.));
#6254=DIRECTION('center_axis',(1.,0.,0.));
#6255=DIRECTION('ref_axis',(0.,1.,0.));
#6256=DIRECTION('center_axis',(1.,0.,0.));
#6257=DIRECTION('ref_axis',(0.,1.,0.));
#6258=DIRECTION('axis',(0.,0.,1.));
#6259=DIRECTION('refdir',(1.,0.,0.));
#6260=DIRECTION('center_axis',(0.,-1.83697019872103E-16,-1.));
#6261=DIRECTION('ref_axis',(0.,-1.,1.83697019872103E-16));
#6262=DIRECTION('center_axis',(0.,1.83697019872103E-16,1.));
#6263=DIRECTION('ref_axis',(0.,-1.,1.83697019872103E-16));
#6264=DIRECTION('center_axis',(-1.,1.22464679914735E-16,-2.24963967399279E-32));
#6265=DIRECTION('ref_axis',(1.22464679914735E-16,1.,-1.83697019872103E-16));
#6266=DIRECTION('center_axis',(0.,1.83697019872103E-16,1.));
#6267=DIRECTION('ref_axis',(0.,-1.,1.83697019872103E-16));
#6268=DIRECTION('center_axis',(0.,-1.83697019872103E-16,-1.));
#6269=DIRECTION('ref_axis',(0.,-1.,1.83697019872103E-16));
#6270=DIRECTION('center_axis',(0.,1.83697019872103E-16,1.));
#6271=DIRECTION('ref_axis',(0.,-1.,1.83697019872103E-16));
#6272=DIRECTION('',(8.65956056235476E-17,0.707106781186533,-0.707106781186562));
#6273=DIRECTION('center_axis',(0.,1.83697019872103E-16,1.));
#6274=DIRECTION('ref_axis',(0.,-1.,1.83697019872103E-16));
#6275=DIRECTION('center_axis',(0.,1.83697019872103E-16,1.));
#6276=DIRECTION('ref_axis',(0.,-1.,1.83697019872103E-16));
#6277=DIRECTION('',(0.,1.83697019872103E-16,1.));
#6278=DIRECTION('center_axis',(0.,1.83697019872103E-16,1.));
#6279=DIRECTION('ref_axis',(0.,-1.,1.83697019872103E-16));
#6280=DIRECTION('center_axis',(0.,1.83697019872103E-16,1.));
#6281=DIRECTION('ref_axis',(0.,-1.,1.83697019872103E-16));
#6282=DIRECTION('center_axis',(0.,1.83697019872103E-16,1.));
#6283=DIRECTION('ref_axis',(0.,1.,-1.83697019872103E-16));
#6284=DIRECTION('',(8.65956056235476E-17,-0.707106781186533,0.707106781186562));
#6285=DIRECTION('center_axis',(0.,1.83697019872103E-16,1.));
#6286=DIRECTION('ref_axis',(0.,-1.,1.83697019872103E-16));
#6287=DIRECTION('center_axis',(0.,1.83697019872103E-16,1.));
#6288=DIRECTION('ref_axis',(0.,-1.,1.83697019872103E-16));
#6289=DIRECTION('center_axis',(0.,1.83697019872103E-16,1.));
#6290=DIRECTION('ref_axis',(0.,-1.,1.83697019872103E-16));
#6291=DIRECTION('',(0.,-1.83697019872103E-16,-1.));
#6292=DIRECTION('center_axis',(0.,1.83697019872103E-16,1.));
#6293=DIRECTION('ref_axis',(0.,-1.,1.83697019872103E-16));
#6294=DIRECTION('',(0.,-1.83697019872103E-16,-1.));
#6295=DIRECTION('center_axis',(0.,1.83697019872103E-16,1.));
#6296=DIRECTION('ref_axis',(0.,-1.,1.83697019872103E-16));
#6297=DIRECTION('center_axis',(0.,-1.83697019872103E-16,-1.));
#6298=DIRECTION('ref_axis',(0.,1.,-1.83697019872103E-16));
#6299=DIRECTION('center_axis',(0.,1.83697019872103E-16,1.));
#6300=DIRECTION('ref_axis',(0.,-1.,1.83697019872103E-16));
#6301=DIRECTION('center_axis',(-1.,0.,0.));
#6302=DIRECTION('ref_axis',(0.,1.,0.));
#6303=DIRECTION('center_axis',(0.,1.22464679914735E-16,1.));
#6304=DIRECTION('ref_axis',(0.,-1.,1.22464679914735E-16));
#6305=DIRECTION('center_axis',(0.,-1.83697019872103E-16,-1.));
#6306=DIRECTION('ref_axis',(0.,-1.,1.83697019872103E-16));
#6307=DIRECTION('center_axis',(0.,1.83697019872103E-16,1.));
#6308=DIRECTION('ref_axis',(0.,-1.,1.83697019872103E-16));
#6309=DIRECTION('',(-8.6595605623548E-17,-0.707106781186537,0.707106781186558));
#6310=DIRECTION('center_axis',(0.,1.83697019872103E-16,1.));
#6311=DIRECTION('ref_axis',(0.,-1.,1.83697019872103E-16));
#6312=DIRECTION('center_axis',(0.,1.83697019872103E-16,1.));
#6313=DIRECTION('ref_axis',(0.,-1.,1.83697019872103E-16));
#6314=DIRECTION('center_axis',(0.,1.83697019872103E-16,1.));
#6315=DIRECTION('ref_axis',(0.,-1.,1.83697019872103E-16));
#6316=DIRECTION('',(0.,1.83697019872103E-16,1.));
#6317=DIRECTION('center_axis',(0.,1.83697019872103E-16,1.));
#6318=DIRECTION('ref_axis',(0.,-1.,1.83697019872103E-16));
#6319=DIRECTION('center_axis',(0.,-1.83697019872103E-16,-1.));
#6320=DIRECTION('ref_axis',(0.,-1.,1.83697019872103E-16));
#6321=DIRECTION('center_axis',(-1.,1.22464679914735E-16,-2.24963967399279E-32));
#6322=DIRECTION('ref_axis',(1.22464679914735E-16,1.,-1.83697019872103E-16));
#6323=DIRECTION('center_axis',(0.,1.83697019872103E-16,1.));
#6324=DIRECTION('ref_axis',(0.,-1.,1.83697019872103E-16));
#6325=DIRECTION('center_axis',(0.,1.83697019872103E-16,1.));
#6326=DIRECTION('ref_axis',(0.,-1.,1.83697019872103E-16));
#6327=DIRECTION('center_axis',(0.,1.83697019872103E-16,1.));
#6328=DIRECTION('ref_axis',(0.,-1.,1.83697019872103E-16));
#6329=DIRECTION('',(0.,1.83697019872103E-16,1.));
#6330=DIRECTION('center_axis',(0.,1.83697019872103E-16,1.));
#6331=DIRECTION('ref_axis',(0.,1.,-1.83697019872103E-16));
#6332=DIRECTION('center_axis',(0.,1.83697019872103E-16,1.));
#6333=DIRECTION('ref_axis',(0.,-1.,1.83697019872103E-16));
#6334=DIRECTION('center_axis',(0.,1.83697019872103E-16,1.));
#6335=DIRECTION('ref_axis',(0.,-1.,1.83697019872103E-16));
#6336=DIRECTION('',(-8.6595605623548E-17,0.707106781186537,-0.707106781186558));
#6337=DIRECTION('center_axis',(0.,1.83697019872103E-16,1.));
#6338=DIRECTION('ref_axis',(0.,-1.,1.83697019872103E-16));
#6339=DIRECTION('center_axis',(0.,1.83697019872103E-16,1.));
#6340=DIRECTION('ref_axis',(0.,-1.,1.83697019872103E-16));
#6341=DIRECTION('',(0.,-1.83697019872103E-16,-1.));
#6342=DIRECTION('center_axis',(0.,-1.83697019872103E-16,-1.));
#6343=DIRECTION('ref_axis',(0.,1.,-1.83697019872103E-16));
#6344=DIRECTION('center_axis',(0.,1.83697019872103E-16,1.));
#6345=DIRECTION('ref_axis',(0.,-1.,1.83697019872103E-16));
#6346=DIRECTION('center_axis',(-0.866025403784438,0.500000000000001,-9.18485099360517E-17));
#6347=DIRECTION('ref_axis',(0.500000000000001,0.866025403784438,2.46107340633671E-17));
#6348=DIRECTION('center_axis',(-3.06161699786839E-17,1.30668257935858E-16,
1.));
#6349=DIRECTION('ref_axis',(-0.500000000000001,-0.866025403784438,9.78539458513683E-17));
#6350=DIRECTION('center_axis',(-0.499999999999998,0.86602540378444,-1.59086285808736E-16));
#6351=DIRECTION('ref_axis',(0.86602540378444,0.499999999999998,9.18485099360519E-17));
#6352=DIRECTION('center_axis',(-5.30287619362453E-17,1.53080849893419E-16,
1.));
#6353=DIRECTION('ref_axis',(-0.86602540378444,-0.499999999999998,3.06161699786834E-17));
#6354=DIRECTION('center_axis',(3.56496022900526E-15,1.,-1.83697019872103E-16));
#6355=DIRECTION('ref_axis',(1.,-3.56496022900527E-15,1.83697019872103E-16));
#6356=DIRECTION('center_axis',(-6.1232339957367E-17,1.83697019872103E-16,
1.));
#6357=DIRECTION('ref_axis',(-1.,3.56496022900527E-15,-6.12323399573677E-17));
#6358=DIRECTION('center_axis',(0.500000000000004,0.866025403784436,-1.59086285808735E-16));
#6359=DIRECTION('ref_axis',(0.866025403784436,-0.500000000000004,2.75545529808155E-16));
#6360=DIRECTION('center_axis',(-5.30287619362453E-17,2.14313189850786E-16,
1.));
#6361=DIRECTION('ref_axis',(-0.866025403784436,0.500000000000004,-1.5308084989342E-16));
#6362=DIRECTION('center_axis',(0.866025403784442,0.499999999999995,-9.18485099360505E-17));
#6363=DIRECTION('ref_axis',(0.499999999999995,-0.866025403784442,3.42783305680839E-16));
#6364=DIRECTION('center_axis',(-3.06161699786832E-17,2.36725781808348E-16,
1.));
#6365=DIRECTION('ref_axis',(-0.499999999999995,0.866025403784442,-2.20318625766104E-16));
#6366=DIRECTION('center_axis',(1.,0.,0.));
#6367=DIRECTION('ref_axis',(0.,-1.,3.67394039744206E-16));
#6368=DIRECTION('center_axis',(0.,2.44929359829471E-16,1.));
#6369=DIRECTION('ref_axis',(0.,1.,-2.44929359829471E-16));
#6370=DIRECTION('center_axis',(0.866025403784434,-0.500000000000008,9.18485099360529E-17));
#6371=DIRECTION('ref_axis',(-0.500000000000008,-0.866025403784434,3.42783305680838E-16));
#6372=DIRECTION('center_axis',(3.06161699786843E-17,2.36725781808348E-16,
1.));
#6373=DIRECTION('ref_axis',(0.500000000000008,0.866025403784434,-2.20318625766103E-16));
#6374=DIRECTION('center_axis',(0.499999999999992,-0.866025403784443,1.59086285808737E-16));
#6375=DIRECTION('ref_axis',(-0.866025403784443,-0.499999999999992,2.75545529808153E-16));
#6376=DIRECTION('center_axis',(5.30287619362456E-17,2.14313189850786E-16,
1.));
#6377=DIRECTION('ref_axis',(0.866025403784443,0.499999999999992,-1.53080849893418E-16));
#6378=DIRECTION('center_axis',(-1.06948806870158E-14,-1.,1.83697019872103E-16));
#6379=DIRECTION('ref_axis',(-1.,1.06948806870158E-14,1.83697019872101E-16));
#6380=DIRECTION('center_axis',(6.12323399573675E-17,1.83697019872102E-16,
1.));
#6381=DIRECTION('ref_axis',(1.,-1.06948806870158E-14,-6.12323399573656E-17));
#6382=DIRECTION('center_axis',(0.,-1.,0.));
#6383=DIRECTION('ref_axis',(0.,0.,-1.));
#6384=DIRECTION('center_axis',(-1.,2.84594884284774E-15,-1.22464679914694E-16));
#6385=DIRECTION('ref_axis',(-1.22464679914735E-16,-1.45251455301593E-14,
1.));
#6386=DIRECTION('center_axis',(0.,-1.,0.));
#6387=DIRECTION('ref_axis',(0.,0.,-1.));
#6388=DIRECTION('center_axis',(1.,0.,-1.22464679914735E-16));
#6389=DIRECTION('ref_axis',(-6.12323399573676E-17,0.,-1.));
#6390=DIRECTION('center_axis',(0.,1.,0.));
#6391=DIRECTION('ref_axis',(6.12323399573676E-17,0.,1.));
#6392=DIRECTION('center_axis',(0.,-1.,0.));
#6393=DIRECTION('ref_axis',(0.,0.,-1.));
#6394=DIRECTION('center_axis',(0.,-1.,0.));
#6395=DIRECTION('ref_axis',(0.,0.,-1.));
#6396=DIRECTION('center_axis',(0.,-1.,0.));
#6397=DIRECTION('ref_axis',(0.,0.,-1.));
#6398=DIRECTION('center_axis',(0.,1.,0.));
#6399=DIRECTION('ref_axis',(0.,0.,1.));
#6400=DIRECTION('center_axis',(-0.500000000000001,-0.866025403784438,-2.46107340633671E-17));
#6401=DIRECTION('ref_axis',(1.23053670316836E-17,2.13135209046589E-17,-1.));
#6402=DIRECTION('center_axis',(-0.866025403784473,0.49999999999994,-4.06043840956678E-14));
#6403=DIRECTION('ref_axis',(0.,8.12087681913454E-14,1.));
#6404=DIRECTION('center_axis',(-0.500000000000001,-0.866025403784438,-2.46107340633671E-17));
#6405=DIRECTION('ref_axis',(1.23053670316836E-17,2.13135209046589E-17,-1.));
#6406=DIRECTION('center_axis',(0.866025403784438,-0.500000000000001,-1.22464679914735E-16));
#6407=DIRECTION('ref_axis',(0.,0.,-1.));
#6408=DIRECTION('center_axis',(0.500000000000001,0.866025403784438,0.));
#6409=DIRECTION('ref_axis',(0.,0.,1.));
#6410=DIRECTION('center_axis',(-0.500000000000001,-0.866025403784438,-2.46107340633671E-17));
#6411=DIRECTION('ref_axis',(1.23053670316836E-17,2.13135209046589E-17,-1.));
#6412=DIRECTION('center_axis',(-0.500000000000001,-0.866025403784438,-2.46107340633671E-17));
#6413=DIRECTION('ref_axis',(1.23053670316836E-17,2.13135209046589E-17,-1.));
#6414=DIRECTION('center_axis',(-0.500000000000001,-0.866025403784438,-2.46107340633671E-17));
#6415=DIRECTION('ref_axis',(9.18485099360517E-17,-2.4610734063367E-17,-1.));
#6416=DIRECTION('center_axis',(0.500000000000001,0.866025403784438,2.46107340633671E-17));
#6417=DIRECTION('ref_axis',(-9.18485099360517E-17,2.4610734063367E-17,1.));
#6418=DIRECTION('center_axis',(-0.86602540378444,-0.499999999999998,-9.18485099360519E-17));
#6419=DIRECTION('ref_axis',(7.95431429043685E-17,4.59242549680258E-17,-1.));
#6420=DIRECTION('center_axis',(0.500000000000015,-0.86602540378443,-9.57339137215078E-15));
#6421=DIRECTION('ref_axis',(-1.9146782744301E-14,0.,-1.));
#6422=DIRECTION('center_axis',(-0.86602540378444,-0.499999999999998,-9.18485099360519E-17));
#6423=DIRECTION('ref_axis',(7.95431429043685E-17,4.59242549680258E-17,-1.));
#6424=DIRECTION('center_axis',(0.499999999999998,-0.86602540378444,-1.22464679914735E-16));
#6425=DIRECTION('ref_axis',(0.,0.,-1.));
#6426=DIRECTION('center_axis',(0.86602540378444,0.499999999999998,0.));
#6427=DIRECTION('ref_axis',(0.,0.,1.));
#6428=DIRECTION('center_axis',(-0.86602540378444,-0.499999999999998,-9.18485099360519E-17));
#6429=DIRECTION('ref_axis',(7.95431429043685E-17,4.59242549680257E-17,-1.));
#6430=DIRECTION('center_axis',(-0.86602540378444,-0.499999999999998,-9.18485099360519E-17));
#6431=DIRECTION('ref_axis',(7.95431429043685E-17,4.59242549680257E-17,-1.));
#6432=DIRECTION('center_axis',(-0.86602540378444,-0.499999999999998,-9.18485099360519E-17));
#6433=DIRECTION('ref_axis',(1.59086285808736E-16,-9.18485099360518E-17,
-1.));
#6434=DIRECTION('center_axis',(0.86602540378444,0.499999999999998,9.18485099360519E-17));
#6435=DIRECTION('ref_axis',(-1.59086285808736E-16,9.18485099360518E-17,
1.));
#6436=DIRECTION('center_axis',(-1.,3.49148133884313E-15,-1.83697019872104E-16));
#6437=DIRECTION('ref_axis',(1.83697019872103E-16,-1.83697019872105E-16,
-1.));
#6438=DIRECTION('center_axis',(-3.56732052431893E-15,-1.,1.22464679914626E-16));
#6439=DIRECTION('ref_axis',(3.03707588357877E-14,-1.22464679914735E-16,
-1.));
#6440=DIRECTION('center_axis',(-1.,3.49148133884313E-15,-1.83697019872104E-16));
#6441=DIRECTION('ref_axis',(1.83697019872103E-16,-1.83697019872105E-16,
-1.));
#6442=DIRECTION('center_axis',(-3.56496022900528E-15,-1.,6.12323399573673E-17));
#6443=DIRECTION('ref_axis',(0.,-1.22464679914736E-16,-1.));
#6444=DIRECTION('center_axis',(1.,-3.56496022900527E-15,4.36581713353893E-31));
#6445=DIRECTION('ref_axis',(0.,1.22464679914736E-16,1.));
#6446=DIRECTION('center_axis',(-1.,3.49148133884313E-15,-1.83697019872104E-16));
#6447=DIRECTION('ref_axis',(1.83697019872103E-16,-1.83697019872104E-16,
-1.));
#6448=DIRECTION('center_axis',(-1.,3.49148133884313E-15,-1.83697019872104E-16));
#6449=DIRECTION('ref_axis',(1.83697019872103E-16,-1.83697019872104E-16,
-1.));
#6450=DIRECTION('center_axis',(-1.,3.49148133884313E-15,-1.83697019872104E-16));
#6451=DIRECTION('ref_axis',(1.83697019872103E-16,-1.83697019872104E-16,
-1.));
#6452=DIRECTION('center_axis',(1.,-3.49148133884313E-15,1.83697019872104E-16));
#6453=DIRECTION('ref_axis',(-1.83697019872103E-16,1.83697019872104E-16,
1.));
#6454=DIRECTION('center_axis',(-0.866025403784436,0.500000000000004,-2.75545529808155E-16));
#6455=DIRECTION('ref_axis',(1.20569152228707E-16,-3.42259162130681E-16,
-1.));
#6456=DIRECTION('center_axis',(-0.499999999999989,-0.866025403784445,-2.60792385655128E-14));
#6457=DIRECTION('ref_axis',(5.21584771310268E-14,0.,-1.));
#6458=DIRECTION('center_axis',(-0.866025403784436,0.500000000000004,-2.75545529808155E-16));
#6459=DIRECTION('ref_axis',(2.5088757443104E-18,-5.46745559357283E-16,-1.));
#6460=DIRECTION('center_axis',(-0.500000000000004,-0.866025403784436,-1.22464679914735E-16));
#6461=DIRECTION('ref_axis',(0.,0.,-1.));
#6462=DIRECTION('center_axis',(0.866025403784436,-0.500000000000004,0.));
#6463=DIRECTION('ref_axis',(0.,0.,1.));
#6464=DIRECTION('center_axis',(-0.866025403784436,0.500000000000004,-2.75545529808155E-16));
#6465=DIRECTION('ref_axis',(1.05327043884768E-16,-3.68659268196852E-16,
-1.));
#6466=DIRECTION('center_axis',(-0.866025403784436,0.500000000000004,-2.75545529808155E-16));
#6467=DIRECTION('ref_axis',(2.38629428713104E-16,-1.37772764904079E-16,
-1.));
#6468=DIRECTION('center_axis',(-0.866025403784436,0.500000000000004,-2.75545529808155E-16));
#6469=DIRECTION('ref_axis',(1.59086285808736E-16,-2.75545529808155E-16,
-1.));
#6470=DIRECTION('center_axis',(0.866025403784436,-0.500000000000004,2.75545529808155E-16));
#6471=DIRECTION('ref_axis',(-1.59086285808736E-16,2.75545529808155E-16,
1.));
#6472=DIRECTION('center_axis',(-0.499999999999995,0.866025403784442,-3.4278330568084E-16));
#6473=DIRECTION('ref_axis',(-6.47289001283727E-17,-4.33183315530548E-16,
-1.));
#6474=DIRECTION('center_axis',(-0.866025403784424,-0.500000000000026,1.08638070651314E-13));
#6475=DIRECTION('ref_axis',(-1.25444438669558E-13,0.,-1.));
#6476=DIRECTION('center_axis',(-0.499999999999995,0.866025403784442,-3.4278330568084E-16));
#6477=DIRECTION('ref_axis',(-6.47289001283722E-17,-4.33183315530548E-16,
-1.));
#6478=DIRECTION('center_axis',(-0.866025403784442,-0.499999999999995,1.67652526221758E-16));
#6479=DIRECTION('ref_axis',(0.,-5.94160038167547E-16,-1.));
#6480=DIRECTION('center_axis',(0.499999999999995,-0.866025403784442,6.43197108708287E-16));
#6481=DIRECTION('ref_axis',(0.,7.42700047709434E-16,1.));
#6482=DIRECTION('center_axis',(-0.499999999999995,0.866025403784442,-3.4278330568084E-16));
#6483=DIRECTION('ref_axis',(-9.52131168162501E-17,-4.50783386241328E-16,
-1.));
#6484=DIRECTION('center_axis',(-0.499999999999995,0.866025403784442,-3.4278330568084E-16));
#6485=DIRECTION('ref_axis',(-9.52131168162501E-17,-4.50783386241328E-16,
-1.));
#6486=DIRECTION('center_axis',(-0.499999999999995,0.866025403784442,-3.4278330568084E-16));
#6487=DIRECTION('ref_axis',(9.18485099360505E-17,-3.4278330568084E-16,-1.));
#6488=DIRECTION('center_axis',(0.499999999999995,-0.866025403784442,3.4278330568084E-16));
#6489=DIRECTION('ref_axis',(-9.18485099360505E-17,3.4278330568084E-16,1.));
#6490=DIRECTION('center_axis',(0.,1.,-3.67394039744206E-16));
#6491=DIRECTION('ref_axis',(0.,-3.67394039744206E-16,-1.));
#6492=DIRECTION('center_axis',(-1.,-7.45578900633689E-15,1.22464679914593E-16));
#6493=DIRECTION('ref_axis',(-1.22464679914735E-16,1.91467827443009E-14,
-1.));
#6494=DIRECTION('center_axis',(0.,1.,-3.67394039744206E-16));
#6495=DIRECTION('ref_axis',(0.,-3.67394039744206E-16,-1.));
#6496=DIRECTION('center_axis',(-1.,0.,-1.22464679914735E-16));
#6497=DIRECTION('ref_axis',(6.12323399573676E-17,0.,-1.));
#6498=DIRECTION('center_axis',(0.,-1.,0.));
#6499=DIRECTION('ref_axis',(-6.12323399573676E-17,0.,1.));
#6500=DIRECTION('center_axis',(0.,1.,-3.67394039744206E-16));
#6501=DIRECTION('ref_axis',(0.,-3.67394039744206E-16,-1.));
#6502=DIRECTION('center_axis',(0.,1.,-3.67394039744206E-16));
#6503=DIRECTION('ref_axis',(0.,-3.67394039744206E-16,-1.));
#6504=DIRECTION('center_axis',(0.,1.,-3.67394039744206E-16));
#6505=DIRECTION('ref_axis',(0.,-3.67394039744206E-16,-1.));
#6506=DIRECTION('center_axis',(0.,-1.,3.67394039744206E-16));
#6507=DIRECTION('ref_axis',(0.,3.67394039744206E-16,1.));
#6508=DIRECTION('center_axis',(0.500000000000007,0.866025403784435,-3.42783305680838E-16));
#6509=DIRECTION('ref_axis',(6.47289001283733E-17,-4.3318331553055E-16,-1.));
#6510=DIRECTION('center_axis',(0.866025403784425,-0.500000000000023,4.66000145162218E-14));
#6511=DIRECTION('ref_axis',(-5.38090618503631E-14,0.,1.));
#6512=DIRECTION('center_axis',(0.500000000000007,0.866025403784435,-3.42783305680838E-16));
#6513=DIRECTION('ref_axis',(6.47289001283733E-17,-4.3318331553055E-16,-1.));
#6514=DIRECTION('center_axis',(-0.866025403784434,0.500000000000007,-4.12581886051237E-16));
#6515=DIRECTION('ref_axis',(0.,-5.94160038167547E-16,-1.));
#6516=DIRECTION('center_axis',(-0.500000000000007,-0.866025403784434,6.43197108708281E-16));
#6517=DIRECTION('ref_axis',(0.,7.42700047709434E-16,1.));
#6518=DIRECTION('center_axis',(0.500000000000007,0.866025403784435,-3.42783305680838E-16));
#6519=DIRECTION('ref_axis',(9.52131168162512E-17,-4.50783386241332E-16,
-1.));
#6520=DIRECTION('center_axis',(0.500000000000007,0.866025403784435,-3.42783305680838E-16));
#6521=DIRECTION('ref_axis',(9.52131168162512E-17,-4.50783386241332E-16,
-1.));
#6522=DIRECTION('center_axis',(0.500000000000007,0.866025403784435,-3.42783305680838E-16));
#6523=DIRECTION('ref_axis',(-9.18485099360527E-17,-3.42783305680838E-16,
-1.));
#6524=DIRECTION('center_axis',(-0.500000000000007,-0.866025403784435,3.42783305680838E-16));
#6525=DIRECTION('ref_axis',(9.18485099360527E-17,3.42783305680838E-16,1.));
#6526=DIRECTION('center_axis',(0.866025403784443,0.499999999999992,-2.75545529808153E-16));
#6527=DIRECTION('ref_axis',(-1.20569152228709E-16,-3.4225916213068E-16,
-1.));
#6528=DIRECTION('center_axis',(0.499999999999992,-0.866025403784443,-2.07973674636369E-14));
#6529=DIRECTION('ref_axis',(4.15947349272745E-14,0.,1.));
#6530=DIRECTION('center_axis',(0.866025403784443,0.499999999999992,-2.75545529808153E-16));
#6531=DIRECTION('ref_axis',(-2.5088757443144E-18,-5.46745559357285E-16,
-1.));
#6532=DIRECTION('center_axis',(-0.499999999999992,0.866025403784443,-1.22464679914735E-16));
#6533=DIRECTION('ref_axis',(0.,0.,-1.));
#6534=DIRECTION('center_axis',(-0.866025403784443,-0.499999999999992,0.));
#6535=DIRECTION('ref_axis',(0.,0.,1.));
#6536=DIRECTION('center_axis',(0.866025403784443,0.499999999999992,-2.75545529808153E-16));
#6537=DIRECTION('ref_axis',(-1.0532704388477E-16,-3.68659268196852E-16,
-1.));
#6538=DIRECTION('center_axis',(0.866025403784443,0.499999999999992,-2.75545529808153E-16));
#6539=DIRECTION('ref_axis',(-2.38629428713104E-16,-1.37772764904074E-16,
-1.));
#6540=DIRECTION('center_axis',(0.866025403784443,0.499999999999992,-2.75545529808153E-16));
#6541=DIRECTION('ref_axis',(-1.59086285808737E-16,-2.75545529808153E-16,
-1.));
#6542=DIRECTION('center_axis',(-0.866025403784443,-0.499999999999992,2.75545529808153E-16));
#6543=DIRECTION('ref_axis',(1.59086285808737E-16,2.75545529808153E-16,1.));
#6544=DIRECTION('center_axis',(1.,-1.04744440165294E-14,-1.83697019872101E-16));
#6545=DIRECTION('ref_axis',(-1.83697019872103E-16,-1.83697019872102E-16,
-1.));
#6546=DIRECTION('center_axis',(-3.12755891751053E-15,-1.,-1.22464679914974E-16));
#6547=DIRECTION('ref_axis',(-7.59268970894693E-14,-1.22464679914737E-16,
1.));
#6548=DIRECTION('center_axis',(1.,-1.04744440165294E-14,-1.83697019872101E-16));
#6549=DIRECTION('ref_axis',(-1.83697019872103E-16,-1.83697019872102E-16,
-1.));
#6550=DIRECTION('center_axis',(1.06948806870158E-14,1.,-3.06161699786834E-16));
#6551=DIRECTION('ref_axis',(0.,-2.44929359829463E-16,-1.));
#6552=DIRECTION('center_axis',(-1.,1.06948806870158E-14,-2.61949028012324E-30));
#6553=DIRECTION('ref_axis',(0.,2.44929359829461E-16,1.));
#6554=DIRECTION('center_axis',(1.,-1.04744440165294E-14,-1.83697019872101E-16));
#6555=DIRECTION('ref_axis',(-1.83697019872103E-16,-1.83697019872101E-16,
-1.));
#6556=DIRECTION('center_axis',(1.,-1.04744440165294E-14,-1.83697019872101E-16));
#6557=DIRECTION('ref_axis',(-1.83697019872103E-16,-1.83697019872101E-16,
-1.));
#6558=DIRECTION('center_axis',(1.,-1.04744440165294E-14,-1.83697019872101E-16));
#6559=DIRECTION('ref_axis',(-1.83697019872103E-16,-1.83697019872101E-16,
-1.));
#6560=DIRECTION('center_axis',(-1.,1.04744440165294E-14,1.83697019872101E-16));
#6561=DIRECTION('ref_axis',(1.83697019872103E-16,1.83697019872101E-16,1.));
#6562=DIRECTION('center_axis',(0.,0.,-1.));
#6563=DIRECTION('ref_axis',(-1.,0.,0.));
#6564=DIRECTION('center_axis',(0.,0.,1.));
#6565=DIRECTION('ref_axis',(1.,0.,0.));
#6566=DIRECTION('',(0.,0.,-1.));
#6567=DIRECTION('center_axis',(0.,0.,1.));
#6568=DIRECTION('ref_axis',(1.,0.,0.));
#6569=DIRECTION('center_axis',(0.,0.,-1.));
#6570=DIRECTION('ref_axis',(-1.,0.,0.));
#6571=DIRECTION('center_axis',(0.,0.,1.));
#6572=DIRECTION('ref_axis',(1.,0.,0.));
#6573=DIRECTION('',(0.,0.,1.));
#6574=DIRECTION('center_axis',(0.,0.,1.));
#6575=DIRECTION('ref_axis',(1.,0.,0.));
#6576=DIRECTION('center_axis',(0.,0.,1.));
#6577=DIRECTION('ref_axis',(1.,0.,0.));
#6578=DIRECTION('center_axis',(0.,0.,1.));
#6579=DIRECTION('ref_axis',(1.,0.,0.));
#6580=DIRECTION('center_axis',(0.866025403784433,-0.50000000000001,-9.18485099360496E-17));
#6581=DIRECTION('ref_axis',(-7.95431429043658E-17,4.59242549680257E-17,
-1.));
#6582=DIRECTION('center_axis',(-0.499999999999991,-0.866025403784444,-6.60233887734503E-16));
#6583=DIRECTION('ref_axis',(-1.32046777546903E-15,0.,1.));
#6584=DIRECTION('center_axis',(0.866025403784433,-0.50000000000001,-9.18485099360496E-17));
#6585=DIRECTION('ref_axis',(-7.95431429043658E-17,4.59242549680257E-17,
-1.));
#6586=DIRECTION('center_axis',(0.50000000000001,0.866025403784433,-1.22464679914735E-16));
#6587=DIRECTION('ref_axis',(0.,0.,-1.));
#6588=DIRECTION('center_axis',(-0.866025403784433,0.50000000000001,0.));
#6589=DIRECTION('ref_axis',(0.,0.,1.));
#6590=DIRECTION('center_axis',(0.866025403784433,-0.50000000000001,-9.18485099360496E-17));
#6591=DIRECTION('ref_axis',(-7.95431429043658E-17,4.59242549680257E-17,
-1.));
#6592=DIRECTION('center_axis',(0.866025403784433,-0.50000000000001,-9.18485099360496E-17));
#6593=DIRECTION('ref_axis',(-7.95431429043658E-17,4.59242549680257E-17,
-1.));
#6594=DIRECTION('center_axis',(0.866025403784433,-0.50000000000001,-9.18485099360497E-17));
#6595=DIRECTION('ref_axis',(-1.59086285808735E-16,-9.18485099360497E-17,
-1.));
#6596=DIRECTION('center_axis',(-0.866025403784433,0.50000000000001,9.18485099360497E-17));
#6597=DIRECTION('ref_axis',(1.59086285808735E-16,9.18485099360497E-17,1.));
#6598=DIRECTION('center_axis',(0.499999999999989,-0.866025403784445,-2.46107340633658E-17));
#6599=DIRECTION('ref_axis',(-1.23053670316826E-17,2.1313520904658E-17,-1.));
#6600=DIRECTION('center_axis',(-0.866025403784448,-0.499999999999983,-1.32046777546899E-15));
#6601=DIRECTION('ref_axis',(0.,-2.64093555093807E-15,1.));
#6602=DIRECTION('center_axis',(0.499999999999989,-0.866025403784445,-2.46107340633658E-17));
#6603=DIRECTION('ref_axis',(-1.23053670316826E-17,2.1313520904658E-17,-1.));
#6604=DIRECTION('center_axis',(0.866025403784445,0.499999999999989,-1.22464679914735E-16));
#6605=DIRECTION('ref_axis',(0.,0.,-1.));
#6606=DIRECTION('center_axis',(-0.499999999999989,0.866025403784445,0.));
#6607=DIRECTION('ref_axis',(0.,0.,1.));
#6608=DIRECTION('center_axis',(0.499999999999989,-0.866025403784445,-2.46107340633658E-17));
#6609=DIRECTION('ref_axis',(-1.23053670316826E-17,2.1313520904658E-17,-1.));
#6610=DIRECTION('center_axis',(0.499999999999989,-0.866025403784445,-2.46107340633658E-17));
#6611=DIRECTION('ref_axis',(-1.23053670316826E-17,2.1313520904658E-17,-1.));
#6612=DIRECTION('center_axis',(0.499999999999989,-0.866025403784445,-2.46107340633658E-17));
#6613=DIRECTION('ref_axis',(-9.18485099360495E-17,-2.46107340633658E-17,
-1.));
#6614=DIRECTION('center_axis',(-0.499999999999989,0.866025403784445,2.46107340633658E-17));
#6615=DIRECTION('ref_axis',(9.18485099360495E-17,2.46107340633658E-17,1.));
#6616=DIRECTION('center_axis',(-0.50000000000001,-0.866025403784433,1.59086285808735E-16));
#6617=DIRECTION('ref_axis',(-0.866025403784433,0.50000000000001,9.18485099360498E-17));
#6618=DIRECTION('center_axis',(5.30287619362451E-17,1.53080849893418E-16,
1.));
#6619=DIRECTION('ref_axis',(0.866025403784433,-0.50000000000001,3.06161699786855E-17));
#6620=DIRECTION('center_axis',(-0.866025403784446,-0.499999999999988,9.18485099360495E-17));
#6621=DIRECTION('ref_axis',(-0.499999999999988,0.866025403784445,2.46107340633657E-17));
#6622=DIRECTION('center_axis',(3.06161699786833E-17,1.30668257935857E-16,
1.));
#6623=DIRECTION('ref_axis',(0.499999999999988,-0.866025403784445,9.78539458513696E-17));
#6624=DIRECTION('center_axis',(0.,1.83697019872103E-16,1.));
#6625=DIRECTION('ref_axis',(0.,1.,-1.78694614991829E-16));
#6626=DIRECTION('center_axis',(0.,-1.83697019872103E-16,-1.));
#6627=DIRECTION('ref_axis',(0.,1.,-1.83697019872103E-16));
#6628=DIRECTION('center_axis',(1.,1.22464679914735E-16,-2.24963967399279E-32));
#6629=DIRECTION('ref_axis',(1.22464679914735E-16,-1.,1.86140223949822E-16));
#6630=DIRECTION('center_axis',(0.,1.83697019872103E-16,1.));
#6631=DIRECTION('ref_axis',(0.,1.,-1.83697019872103E-16));
#6632=DIRECTION('center_axis',(0.,1.83697019872103E-16,1.));
#6633=DIRECTION('ref_axis',(0.,1.,-1.83697019872103E-16));
#6634=DIRECTION('center_axis',(0.,1.83697019872103E-16,1.));
#6635=DIRECTION('ref_axis',(0.,1.,-1.95204048285742E-16));
#6636=DIRECTION('center_axis',(0.,-1.83697019872103E-16,-1.));
#6637=DIRECTION('ref_axis',(0.,1.,-1.83697019872103E-16));
#6638=DIRECTION('center_axis',(1.,1.22464679914735E-16,-2.24963967399279E-32));
#6639=DIRECTION('ref_axis',(1.22464679914735E-16,-1.,1.83003795267883E-16));
#6640=DIRECTION('center_axis',(0.,1.83697019872103E-16,1.));
#6641=DIRECTION('ref_axis',(0.,1.,-1.83697019872103E-16));
#6642=DIRECTION('center_axis',(0.,-1.83697019872103E-16,-1.));
#6643=DIRECTION('ref_axis',(0.,1.,-1.83697019872103E-16));
#6644=DIRECTION('center_axis',(0.,1.83697019872103E-16,1.));
#6645=DIRECTION('ref_axis',(0.,-1.,1.83697019872103E-16));
#6646=DIRECTION('center_axis',(0.,1.83697019872103E-16,1.));
#6647=DIRECTION('ref_axis',(0.,-1.,1.83697019872103E-16));
#6648=DIRECTION('center_axis',(0.,1.83697019872103E-16,1.));
#6649=DIRECTION('ref_axis',(0.,-1.,1.83697019872103E-16));
#6650=DIRECTION('',(0.,-1.83697019872103E-16,-1.));
#6651=DIRECTION('center_axis',(0.,1.83697019872103E-16,1.));
#6652=DIRECTION('ref_axis',(0.,1.,-1.83697019872103E-16));
#6653=DIRECTION('center_axis',(0.,1.83697019872103E-16,1.));
#6654=DIRECTION('ref_axis',(0.,-1.,1.83697019872103E-16));
#6655=DIRECTION('',(-1.0420961835668E-16,0.850936110144042,-0.525269203792614));
#6656=DIRECTION('center_axis',(0.,-1.83697019872103E-16,-1.));
#6657=DIRECTION('ref_axis',(0.,-1.,1.83697019872103E-16));
#6658=DIRECTION('center_axis',(0.,1.83697019872103E-16,1.));
#6659=DIRECTION('ref_axis',(0.,-1.,1.83697019872103E-16));
#6660=DIRECTION('',(1.0420961835668E-16,0.850936110144042,-0.525269203792614));
#6661=DIRECTION('center_axis',(0.,1.83697019872103E-16,1.));
#6662=DIRECTION('ref_axis',(0.,-1.,1.83697019872103E-16));
#6663=DIRECTION('center_axis',(0.,1.83697019872103E-16,1.));
#6664=DIRECTION('ref_axis',(0.,-1.,1.83697019872103E-16));
#6665=DIRECTION('',(0.,1.83697019872103E-16,1.));
#6666=DIRECTION('center_axis',(0.,-1.83697019872103E-16,-1.));
#6667=DIRECTION('ref_axis',(0.,1.,-1.83697019872103E-16));
#6668=DIRECTION('center_axis',(0.,1.83697019872103E-16,1.));
#6669=DIRECTION('ref_axis',(0.,-1.,1.83697019872103E-16));
#6670=DIRECTION('center_axis',(0.,-1.83697019872103E-16,-1.));
#6671=DIRECTION('ref_axis',(0.,-1.,1.95204048285742E-16));
#6672=DIRECTION('center_axis',(0.,1.83697019872103E-16,1.));
#6673=DIRECTION('ref_axis',(0.,-1.,1.83697019872103E-16));
#6674=DIRECTION('center_axis',(1.,-1.22464679914735E-16,2.24963967399279E-32));
#6675=DIRECTION('ref_axis',(1.22464679914735E-16,1.,-1.83003795267883E-16));
#6676=DIRECTION('center_axis',(0.,-1.83697019872103E-16,-1.));
#6677=DIRECTION('ref_axis',(0.,-1.,1.83697019872103E-16));
#6678=DIRECTION('center_axis',(0.,-1.83697019872103E-16,-1.));
#6679=DIRECTION('ref_axis',(0.,-1.,1.78694614991829E-16));
#6680=DIRECTION('center_axis',(0.,1.83697019872103E-16,1.));
#6681=DIRECTION('ref_axis',(0.,-1.,1.83697019872103E-16));
#6682=DIRECTION('center_axis',(1.,-1.22464679914735E-16,2.24963967399279E-32));
#6683=DIRECTION('ref_axis',(1.22464679914735E-16,1.,-1.86140223949822E-16));
#6684=DIRECTION('center_axis',(0.,-1.83697019872103E-16,-1.));
#6685=DIRECTION('ref_axis',(0.,-1.,1.83697019872103E-16));
#6686=DIRECTION('center_axis',(0.,1.83697019872103E-16,1.));
#6687=DIRECTION('ref_axis',(0.,-1.,1.83697019872103E-16));
#6688=DIRECTION('center_axis',(0.,1.83697019872103E-16,1.));
#6689=DIRECTION('ref_axis',(0.,-1.,1.83697019872103E-16));
#6690=DIRECTION('center_axis',(0.,1.83697019872103E-16,1.));
#6691=DIRECTION('ref_axis',(0.,-1.,1.83697019872103E-16));
#6692=DIRECTION('',(0.,1.83697019872103E-16,1.));
#6693=DIRECTION('center_axis',(0.,1.83697019872103E-16,1.));
#6694=DIRECTION('ref_axis',(0.,1.,-1.83697019872103E-16));
#6695=DIRECTION('center_axis',(0.,1.83697019872103E-16,1.));
#6696=DIRECTION('ref_axis',(0.,-1.,1.83697019872103E-16));
#6697=DIRECTION('',(1.0420961835668E-16,-0.850936110144042,0.525269203792614));
#6698=DIRECTION('center_axis',(0.,-1.83697019872103E-16,-1.));
#6699=DIRECTION('ref_axis',(0.,-1.,1.83697019872103E-16));
#6700=DIRECTION('center_axis',(0.,1.83697019872103E-16,1.));
#6701=DIRECTION('ref_axis',(0.,-1.,1.83697019872103E-16));
#6702=DIRECTION('',(-1.0420961835668E-16,-0.850936110144042,0.525269203792614));
#6703=DIRECTION('center_axis',(0.,1.83697019872103E-16,1.));
#6704=DIRECTION('ref_axis',(0.,-1.,1.83697019872103E-16));
#6705=DIRECTION('center_axis',(0.,1.83697019872103E-16,1.));
#6706=DIRECTION('ref_axis',(0.,-1.,1.83697019872103E-16));
#6707=DIRECTION('',(0.,-1.83697019872103E-16,-1.));
#6708=DIRECTION('center_axis',(0.,-1.83697019872103E-16,-1.));
#6709=DIRECTION('ref_axis',(0.,1.,-1.83697019872103E-16));
#6710=DIRECTION('center_axis',(0.,1.83697019872103E-16,1.));
#6711=DIRECTION('ref_axis',(0.,-1.,1.83697019872103E-16));
#6712=DIRECTION('axis',(0.,0.,1.));
#6713=DIRECTION('refdir',(1.,0.,0.));
#6714=DIRECTION('center_axis',(0.,0.,1.));
#6715=DIRECTION('ref_axis',(-1.,0.,0.));
#6716=DIRECTION('center_axis',(-2.32004514166519E-15,0.,1.));
#6717=DIRECTION('ref_axis',(-1.,0.,-2.32004514166519E-15));
#6718=DIRECTION('',(-0.739271628119017,-9.05346633076407E-17,-0.673407350611988));
#6719=DIRECTION('center_axis',(2.32004514166519E-15,0.,-1.));
#6720=DIRECTION('ref_axis',(-1.,0.,-2.32004514166519E-15));
#6721=DIRECTION('center_axis',(2.32004514166519E-15,0.,-1.));
#6722=DIRECTION('ref_axis',(-1.,0.,-2.30926389122043E-15));
#6723=DIRECTION('center_axis',(-2.32004514166519E-15,0.,1.));
#6724=DIRECTION('ref_axis',(1.,0.,2.32004514166519E-15));
#6725=DIRECTION('center_axis',(-1.22464679914735E-16,-1.,-2.84123585661764E-31));
#6726=DIRECTION('ref_axis',(1.,-1.22464679914735E-16,2.22044604925042E-15));
#6727=DIRECTION('center_axis',(2.32004514166519E-15,0.,-1.));
#6728=DIRECTION('ref_axis',(1.,0.,2.32004514166519E-15));
#6729=DIRECTION('center_axis',(-2.32004514166519E-15,0.,1.));
#6730=DIRECTION('ref_axis',(1.,0.,2.32004514166519E-15));
#6731=DIRECTION('',(-0.866025403784439,-0.5,-2.00921803060872E-15));
#6732=DIRECTION('',(-0.866025403784439,0.5,-2.00921803060872E-15));
#6733=DIRECTION('',(7.69185074553425E-16,1.,1.78454409525905E-30));
#6734=DIRECTION('',(0.866025403784439,0.5,2.00921803060872E-15));
#6735=DIRECTION('',(0.866025403784438,-0.5,2.00921803060872E-15));
#6736=DIRECTION('',(0.,-1.,0.));
#6737=DIRECTION('center_axis',(2.32004514166519E-15,0.,-1.));
#6738=DIRECTION('ref_axis',(-1.,0.,-2.32004514166519E-15));
#6739=DIRECTION('center_axis',(2.32004514166519E-15,0.,-1.));
#6740=DIRECTION('ref_axis',(1.,0.,2.32004514166519E-15));
#6741=DIRECTION('',(-2.32004514166519E-15,0.,1.));
#6742=DIRECTION('center_axis',(0.0435778713738291,-0.0754790873051733,-0.996194698091746));
#6743=DIRECTION('ref_axis',(-0.866025403784439,-0.5,-3.35810244624808E-17));
#6744=DIRECTION('',(1.59381164582915E-16,0.997141949694316,-0.0755508581011305));
#6745=DIRECTION('',(-0.866025403784439,-0.5,0.));
#6746=DIRECTION('',(-0.863550259614423,0.498570974847158,-0.0755508581011305));
#6747=DIRECTION('center_axis',(0.0871557427476581,0.,-0.996194698091746));
#6748=DIRECTION('ref_axis',(0.,-1.,0.));
#6749=DIRECTION('',(0.,-1.,0.));
#6750=DIRECTION('',(-0.863550259614423,-0.498570974847158,-0.0755508581011305));
#6751=DIRECTION('center_axis',(0.0435778713738291,0.0754790873051733,-0.996194698091746));
#6752=DIRECTION('ref_axis',(0.866025403784438,-0.5,-8.05233896096258E-18));
#6753=DIRECTION('',(0.866025403784438,-0.5,0.));
#6754=DIRECTION('',(-1.59381164582915E-16,-0.997141949694316,-0.0755508581011305));
#6755=DIRECTION('center_axis',(-0.0435778713738291,0.0754790873051733,-0.996194698091746));
#6756=DIRECTION('ref_axis',(0.866025403784439,0.5,-3.35810244624808E-17));
#6757=DIRECTION('',(0.866025403784439,0.5,0.));
#6758=DIRECTION('',(0.863550259614423,-0.498570974847159,-0.0755508581011306));
#6759=DIRECTION('center_axis',(-0.0871557427476581,6.70388964831166E-17,
-0.996194698091746));
#6760=DIRECTION('ref_axis',(7.69185074553425E-16,1.,7.59804895741788E-32));
#6761=DIRECTION('',(7.69185074553425E-16,1.,0.));
#6762=DIRECTION('',(0.863550259614423,0.498570974847158,-0.0755508581011305));
#6763=DIRECTION('center_axis',(-0.0435778713738291,-0.0754790873051733,
-0.996194698091746));
#6764=DIRECTION('ref_axis',(-0.866025403784439,0.5,3.35810244624808E-17));
#6765=DIRECTION('',(-0.866025403784439,0.5,0.));
#6766=DIRECTION('center_axis',(0.5,-0.866025403784439,0.));
#6767=DIRECTION('ref_axis',(-0.866025403784439,-0.5,0.));
#6768=DIRECTION('',(0.,0.,-1.));
#6769=DIRECTION('',(0.,0.,-1.));
#6770=DIRECTION('center_axis',(1.,0.,0.));
#6771=DIRECTION('ref_axis',(0.,-1.,0.));
#6772=DIRECTION('',(0.,0.,-1.));
#6773=DIRECTION('center_axis',(0.5,0.866025403784438,0.));
#6774=DIRECTION('ref_axis',(0.866025403784438,-0.5,0.));
#6775=DIRECTION('',(0.,0.,-1.));
#6776=DIRECTION('center_axis',(-0.5,0.866025403784439,0.));
#6777=DIRECTION('ref_axis',(0.866025403784439,0.5,0.));
#6778=DIRECTION('',(0.,0.,-1.));
#6779=DIRECTION('center_axis',(-1.,7.69185074553425E-16,0.));
#6780=DIRECTION('ref_axis',(7.69185074553425E-16,1.,0.));
#6781=DIRECTION('',(0.,0.,-1.));
#6782=DIRECTION('center_axis',(-0.5,-0.866025403784439,0.));
#6783=DIRECTION('ref_axis',(-0.866025403784439,0.5,0.));
#6784=DIRECTION('center_axis',(2.32004514166519E-15,0.,-1.));
#6785=DIRECTION('ref_axis',(-1.,0.,-2.32004514166519E-15));
#6786=DIRECTION('',(-2.32004514166519E-15,0.,1.));
#6787=DIRECTION('center_axis',(-2.32004514166519E-15,0.,1.));
#6788=DIRECTION('ref_axis',(-1.,0.,-2.32004514166519E-15));
#6789=DIRECTION('center_axis',(2.32004514166519E-15,0.,-1.));
#6790=DIRECTION('ref_axis',(-1.,0.,-2.32004514166519E-15));
#6791=DIRECTION('center_axis',(2.32004514166519E-15,0.,-1.));
#6792=DIRECTION('ref_axis',(-1.,0.,-2.32004514166519E-15));
#6793=DIRECTION('axis',(0.,0.,1.));
#6794=DIRECTION('refdir',(1.,0.,0.));
#6795=DIRECTION('center_axis',(1.,0.,0.));
#6796=DIRECTION('ref_axis',(0.,-1.,0.));
#6797=DIRECTION('center_axis',(1.,0.,0.));
#6798=DIRECTION('ref_axis',(0.,-1.,0.));
#6799=DIRECTION('',(1.,0.,0.));
#6800=DIRECTION('center_axis',(1.,0.,0.));
#6801=DIRECTION('ref_axis',(0.,-1.,0.));
#6802=DIRECTION('center_axis',(-1.,0.,0.));
#6803=DIRECTION('ref_axis',(0.,-1.,0.));
#6804=DIRECTION('center_axis',(-1.,0.,0.));
#6805=DIRECTION('ref_axis',(0.,1.,0.));
#6806=DIRECTION('center_axis',(-1.,0.,0.));
#6807=DIRECTION('ref_axis',(0.,1.,0.));
#6808=DIRECTION('',(-1.,0.,0.));
#6809=DIRECTION('center_axis',(-1.,0.,0.));
#6810=DIRECTION('ref_axis',(0.,1.,0.));
#6811=DIRECTION('center_axis',(1.,0.,0.));
#6812=DIRECTION('ref_axis',(0.,1.,0.));
#6813=DIRECTION('center_axis',(-1.,0.,0.));
#6814=DIRECTION('ref_axis',(0.,-1.,0.));
#6815=DIRECTION('center_axis',(1.,0.,0.));
#6816=DIRECTION('ref_axis',(0.,-1.,0.));
#6817=DIRECTION('center_axis',(-1.,0.,0.));
#6818=DIRECTION('ref_axis',(0.,-1.,0.));
#6819=DIRECTION('',(1.,0.,0.));
#6820=DIRECTION('center_axis',(-1.,0.,0.));
#6821=DIRECTION('ref_axis',(0.,-1.,0.));
#6822=DIRECTION('center_axis',(-1.,0.,0.));
#6823=DIRECTION('ref_axis',(0.,-1.,0.));
#6824=DIRECTION('axis',(0.,0.,1.));
#6825=DIRECTION('refdir',(1.,0.,0.));
#6826=DIRECTION('center_axis',(1.,0.,0.));
#6827=DIRECTION('ref_axis',(0.,1.,0.));
#6828=DIRECTION('center_axis',(-1.,0.,0.));
#6829=DIRECTION('ref_axis',(0.,1.,0.));
#6830=DIRECTION('center_axis',(1.,0.,0.));
#6831=DIRECTION('ref_axis',(0.,1.,0.));
#6832=DIRECTION('center_axis',(1.,0.,0.));
#6833=DIRECTION('ref_axis',(0.,1.,0.));
#6834=DIRECTION('',(-1.,0.,0.));
#6835=DIRECTION('center_axis',(1.,0.,0.));
#6836=DIRECTION('ref_axis',(0.,1.,0.));
#6837=DIRECTION('axis',(0.,0.,1.));
#6838=DIRECTION('refdir',(1.,0.,0.));
#6839=DIRECTION('center_axis',(1.,0.,0.));
#6840=DIRECTION('ref_axis',(0.,-1.,0.));
#6841=DIRECTION('center_axis',(1.,0.,0.));
#6842=DIRECTION('ref_axis',(0.,-1.,0.));
#6843=DIRECTION('',(1.,0.,0.));
#6844=DIRECTION('center_axis',(1.,0.,0.));
#6845=DIRECTION('ref_axis',(0.,-1.,0.));
#6846=DIRECTION('center_axis',(-1.,0.,0.));
#6847=DIRECTION('ref_axis',(0.,-1.,0.));
#6848=DIRECTION('center_axis',(-1.,0.,0.));
#6849=DIRECTION('ref_axis',(0.,1.,0.));
#6850=DIRECTION('center_axis',(-1.,0.,0.));
#6851=DIRECTION('ref_axis',(0.,1.,0.));
#6852=DIRECTION('',(-1.,0.,0.));
#6853=DIRECTION('center_axis',(-1.,0.,0.));
#6854=DIRECTION('ref_axis',(0.,1.,0.));
#6855=DIRECTION('center_axis',(1.,0.,0.));
#6856=DIRECTION('ref_axis',(0.,1.,0.));
#6857=DIRECTION('center_axis',(1.,0.,0.));
#6858=DIRECTION('ref_axis',(0.,1.,0.));
#6859=DIRECTION('center_axis',(-1.,0.,0.));
#6860=DIRECTION('ref_axis',(0.,1.,0.));
#6861=DIRECTION('center_axis',(1.,0.,0.));
#6862=DIRECTION('ref_axis',(0.,1.,0.));
#6863=DIRECTION('center_axis',(1.,0.,0.));
#6864=DIRECTION('ref_axis',(0.,1.,0.));
#6865=DIRECTION('',(-1.,0.,0.));
#6866=DIRECTION('center_axis',(1.,0.,0.));
#6867=DIRECTION('ref_axis',(0.,1.,0.));
#6868=DIRECTION('axis',(0.,0.,1.));
#6869=DIRECTION('refdir',(1.,0.,0.));
#6870=DIRECTION('center_axis',(0.,-1.83697019872103E-16,1.));
#6871=DIRECTION('ref_axis',(0.,-1.,-1.83697019872103E-16));
#6872=DIRECTION('center_axis',(0.,-1.83697019872103E-16,1.));
#6873=DIRECTION('ref_axis',(0.,-1.,-1.83697019872103E-16));
#6874=DIRECTION('center_axis',(1.,1.22464679914735E-16,2.24963967399279E-32));
#6875=DIRECTION('ref_axis',(-1.22464679914735E-16,1.,1.83697019872103E-16));
#6876=DIRECTION('center_axis',(0.,-1.83697019872103E-16,1.));
#6877=DIRECTION('ref_axis',(0.,-1.,-1.83697019872103E-16));
#6878=DIRECTION('center_axis',(0.,-1.83697019872103E-16,1.));
#6879=DIRECTION('ref_axis',(0.,-1.,-1.83697019872103E-16));
#6880=DIRECTION('center_axis',(0.,-1.83697019872103E-16,1.));
#6881=DIRECTION('ref_axis',(0.,-1.,-1.83697019872103E-16));
#6882=DIRECTION('',(-8.65956056235486E-17,0.707106781186541,0.707106781186554));
#6883=DIRECTION('center_axis',(0.,-1.83697019872103E-16,1.));
#6884=DIRECTION('ref_axis',(0.,-1.,-1.83697019872103E-16));
#6885=DIRECTION('center_axis',(0.,-1.83697019872103E-16,1.));
#6886=DIRECTION('ref_axis',(0.,-1.,-1.83697019872103E-16));
#6887=DIRECTION('center_axis',(0.,-1.83697019872103E-16,1.));
#6888=DIRECTION('ref_axis',(0.,-1.,-1.83697019872103E-16));
#6889=DIRECTION('center_axis',(0.,-1.83697019872103E-16,1.));
#6890=DIRECTION('ref_axis',(0.,-1.,-1.83697019872103E-16));
#6891=DIRECTION('',(0.,-1.83697019872103E-16,1.));
#6892=DIRECTION('center_axis',(0.,1.83697019872103E-16,-1.));
#6893=DIRECTION('ref_axis',(0.,1.,1.83697019872103E-16));
#6894=DIRECTION('',(-8.65956056235486E-17,-0.707106781186541,-0.707106781186554));
#6895=DIRECTION('center_axis',(0.,-1.83697019872103E-16,1.));
#6896=DIRECTION('ref_axis',(0.,-1.,-1.83697019872103E-16));
#6897=DIRECTION('center_axis',(0.,-1.83697019872103E-16,1.));
#6898=DIRECTION('ref_axis',(0.,-1.,-1.83697019872103E-16));
#6899=DIRECTION('',(0.,1.83697019872103E-16,-1.));
#6900=DIRECTION('center_axis',(0.,-1.83697019872103E-16,1.));
#6901=DIRECTION('ref_axis',(0.,-1.,-1.83697019872103E-16));
#6902=DIRECTION('center_axis',(0.,-1.83697019872103E-16,1.));
#6903=DIRECTION('ref_axis',(0.,-1.,-1.83697019872103E-16));
#6904=DIRECTION('center_axis',(0.,-1.83697019872103E-16,1.));
#6905=DIRECTION('ref_axis',(0.,-1.,-1.83697019872103E-16));
#6906=DIRECTION('',(0.,1.83697019872103E-16,-1.));
#6907=DIRECTION('center_axis',(0.,1.83697019872103E-16,-1.));
#6908=DIRECTION('ref_axis',(0.,1.,1.83697019872103E-16));
#6909=DIRECTION('center_axis',(0.,-1.83697019872103E-16,1.));
#6910=DIRECTION('ref_axis',(0.,-1.,-1.83697019872103E-16));
#6911=DIRECTION('center_axis',(-1.,0.,0.));
#6912=DIRECTION('ref_axis',(0.,1.,0.));
#6913=DIRECTION('center_axis',(0.,1.22464679914735E-16,1.));
#6914=DIRECTION('ref_axis',(0.,-1.,1.22464679914735E-16));
#6915=DIRECTION('center_axis',(0.,-1.83697019872103E-16,1.));
#6916=DIRECTION('ref_axis',(0.,-1.,-1.83697019872103E-16));
#6917=DIRECTION('center_axis',(0.,-1.83697019872103E-16,1.));
#6918=DIRECTION('ref_axis',(0.,-1.,-1.83697019872103E-16));
#6919=DIRECTION('',(8.65956056235492E-17,-0.707106781186546,-0.707106781186549));
#6920=DIRECTION('center_axis',(0.,-1.83697019872103E-16,1.));
#6921=DIRECTION('ref_axis',(0.,-1.,-1.83697019872103E-16));
#6922=DIRECTION('center_axis',(0.,-1.83697019872103E-16,1.));
#6923=DIRECTION('ref_axis',(0.,-1.,-1.83697019872103E-16));
#6924=DIRECTION('center_axis',(0.,-1.83697019872103E-16,1.));
#6925=DIRECTION('ref_axis',(0.,-1.,-1.83697019872103E-16));
#6926=DIRECTION('',(0.,-1.83697019872103E-16,1.));
#6927=DIRECTION('center_axis',(0.,-1.83697019872103E-16,1.));
#6928=DIRECTION('ref_axis',(0.,-1.,-1.83697019872103E-16));
#6929=DIRECTION('center_axis',(0.,-1.83697019872103E-16,1.));
#6930=DIRECTION('ref_axis',(0.,-1.,-1.83697019872103E-16));
#6931=DIRECTION('center_axis',(1.,1.22464679914735E-16,2.24963967399279E-32));
#6932=DIRECTION('ref_axis',(-1.22464679914735E-16,1.,1.83697019872103E-16));
#6933=DIRECTION('center_axis',(0.,-1.83697019872103E-16,1.));
#6934=DIRECTION('ref_axis',(0.,-1.,-1.83697019872103E-16));
#6935=DIRECTION('center_axis',(0.,-1.83697019872103E-16,1.));
#6936=DIRECTION('ref_axis',(0.,-1.,-1.83697019872103E-16));
#6937=DIRECTION('',(0.,-1.83697019872103E-16,1.));
#6938=DIRECTION('center_axis',(0.,-1.83697019872103E-16,1.));
#6939=DIRECTION('ref_axis',(0.,-1.,-1.83697019872103E-16));
#6940=DIRECTION('center_axis',(0.,1.83697019872103E-16,-1.));
#6941=DIRECTION('ref_axis',(0.,1.,1.83697019872103E-16));
#6942=DIRECTION('center_axis',(0.,-1.83697019872103E-16,1.));
#6943=DIRECTION('ref_axis',(0.,-1.,-1.83697019872103E-16));
#6944=DIRECTION('',(8.65956056235491E-17,0.707106781186546,0.707106781186549));
#6945=DIRECTION('center_axis',(0.,-1.83697019872103E-16,1.));
#6946=DIRECTION('ref_axis',(0.,-1.,-1.83697019872103E-16));
#6947=DIRECTION('center_axis',(0.,-1.83697019872103E-16,1.));
#6948=DIRECTION('ref_axis',(0.,-1.,-1.83697019872103E-16));
#6949=DIRECTION('center_axis',(0.,-1.83697019872103E-16,1.));
#6950=DIRECTION('ref_axis',(0.,-1.,-1.83697019872103E-16));
#6951=DIRECTION('',(0.,1.83697019872103E-16,-1.));
#6952=DIRECTION('center_axis',(0.,1.83697019872103E-16,-1.));
#6953=DIRECTION('ref_axis',(0.,1.,1.83697019872103E-16));
#6954=DIRECTION('center_axis',(0.,-1.83697019872103E-16,1.));
#6955=DIRECTION('ref_axis',(0.,-1.,-1.83697019872103E-16));
#6956=DIRECTION('center_axis',(-0.707106781186546,0.707106781186549,1.29893408435324E-16));
#6957=DIRECTION('ref_axis',(0.707106781186549,0.707106781186546,-5.38036114367792E-17));
#6958=DIRECTION('center_axis',(2.16489014058874E-16,3.279199418677E-17,
1.));
#6959=DIRECTION('ref_axis',(-0.707106781186549,-0.707106781186546,1.76268291351515E-16));
#6960=DIRECTION('center_axis',(3.71625375700965E-15,1.,1.83697019872103E-16));
#6961=DIRECTION('ref_axis',(1.,-3.71625375700965E-15,-1.83697019872104E-16));
#6962=DIRECTION('center_axis',(3.06161699786839E-16,-1.83697019872104E-16,
1.));
#6963=DIRECTION('ref_axis',(-1.,3.71625375700965E-15,3.06161699786839E-16));
#6964=DIRECTION('center_axis',(0.707106781186551,0.707106781186544,1.29893408435323E-16));
#6965=DIRECTION('ref_axis',(0.707106781186544,-0.707106781186551,-3.13590428307427E-16));
#6966=DIRECTION('center_axis',(2.16489014058872E-16,-4.00186033930977E-16,
1.));
#6967=DIRECTION('ref_axis',(-0.707106781186544,0.707106781186551,4.36055108222162E-16));
#6968=DIRECTION('center_axis',(1.,0.,0.));
#6969=DIRECTION('ref_axis',(0.,-1.,-3.67394039744206E-16));
#6970=DIRECTION('center_axis',(0.,-4.89858719658941E-16,1.));
#6971=DIRECTION('ref_axis',(0.,1.,4.89858719658941E-16));
#6972=DIRECTION('center_axis',(0.707106781186541,-0.707106781186554,-1.29893408435325E-16));
#6973=DIRECTION('ref_axis',(-0.707106781186554,-0.707106781186541,-3.13590428307426E-16));
#6974=DIRECTION('center_axis',(-2.16489014058876E-16,-4.00186033930974E-16,
1.));
#6975=DIRECTION('ref_axis',(0.707106781186554,0.707106781186541,4.36055108222162E-16));
#6976=DIRECTION('center_axis',(-1.05293856448607E-14,-1.,-1.83697019872103E-16));
#6977=DIRECTION('ref_axis',(-1.,1.05293856448607E-14,-1.83697019872101E-16));
#6978=DIRECTION('center_axis',(-3.06161699786838E-16,-1.836970198721E-16,
1.));
#6979=DIRECTION('ref_axis',(1.,-1.05293856448607E-14,3.06161699786836E-16));
#6980=DIRECTION('center_axis',(-0.707106781186556,-0.707106781186539,-1.29893408435322E-16));
#6981=DIRECTION('ref_axis',(-0.707106781186539,0.707106781186556,-5.38036114367774E-17));
#6982=DIRECTION('center_axis',(-2.1648901405887E-16,3.27919941867732E-17,
1.));
#6983=DIRECTION('ref_axis',(0.707106781186539,-0.707106781186556,1.76268291351513E-16));
#6984=DIRECTION('center_axis',(0.,1.,0.));
#6985=DIRECTION('ref_axis',(0.,0.,1.));
#6986=DIRECTION('center_axis',(0.,1.,0.));
#6987=DIRECTION('ref_axis',(0.,0.,1.));
#6988=DIRECTION('center_axis',(-1.,0.,1.22464679914735E-16));
#6989=DIRECTION('ref_axis',(-1.22464679914735E-16,0.,-1.));
#6990=DIRECTION('center_axis',(0.,1.,0.));
#6991=DIRECTION('ref_axis',(0.,0.,1.));
#6992=DIRECTION('center_axis',(1.,0.,1.22464679914734E-16));
#6993=DIRECTION('ref_axis',(-6.12323399573672E-17,0.,1.));
#6994=DIRECTION('center_axis',(0.,-1.,0.));
#6995=DIRECTION('ref_axis',(6.12323399573672E-17,0.,-1.));
#6996=DIRECTION('center_axis',(0.,1.,0.));
#6997=DIRECTION('ref_axis',(0.,0.,1.));
#6998=DIRECTION('center_axis',(0.,1.,0.));
#6999=DIRECTION('ref_axis',(0.,0.,1.));
#7000=DIRECTION('center_axis',(0.,1.,0.));
#7001=DIRECTION('ref_axis',(0.,0.,1.));
#7002=DIRECTION('center_axis',(0.,-1.,0.));
#7003=DIRECTION('ref_axis',(0.,0.,-1.));
#7004=DIRECTION('center_axis',(0.707106781186549,0.707106781186546,-5.38036114367792E-17));
#7005=DIRECTION('ref_axis',(0.,0.,1.));
#7006=DIRECTION('center_axis',(0.707106781186549,0.707106781186546,-5.38036114367792E-17));
#7007=DIRECTION('ref_axis',(3.80448984992727E-17,3.80448984992726E-17,1.));
#7008=DIRECTION('center_axis',(-0.707106781186546,0.707106781186549,0.));
#7009=DIRECTION('ref_axis',(0.,0.,-1.));
#7010=DIRECTION('center_axis',(0.707106781186549,0.707106781186546,-5.38036114367792E-17));
#7011=DIRECTION('ref_axis',(3.80448984992727E-17,3.80448984992726E-17,1.));
#7012=DIRECTION('center_axis',(0.707106781186546,-0.707106781186549,1.22464679914734E-16));
#7013=DIRECTION('ref_axis',(0.,0.,1.));
#7014=DIRECTION('center_axis',(-0.707106781186549,-0.707106781186546,0.));
#7015=DIRECTION('ref_axis',(0.,0.,-1.));
#7016=DIRECTION('center_axis',(0.707106781186549,0.707106781186546,-5.38036114367792E-17));
#7017=DIRECTION('ref_axis',(3.80448984992727E-17,3.80448984992726E-17,1.));
#7018=DIRECTION('center_axis',(0.707106781186549,0.707106781186546,-5.38036114367792E-17));
#7019=DIRECTION('ref_axis',(3.80448984992727E-17,3.80448984992726E-17,1.));
#7020=DIRECTION('center_axis',(0.707106781186549,0.707106781186546,-5.38036114367792E-17));
#7021=DIRECTION('ref_axis',(1.29893408435324E-16,-5.38036114367791E-17,
1.));
#7022=DIRECTION('center_axis',(-0.707106781186549,-0.707106781186546,5.38036114367792E-17));
#7023=DIRECTION('ref_axis',(-1.29893408435324E-16,5.38036114367791E-17,
-1.));
#7024=DIRECTION('center_axis',(1.,-3.49148133884313E-15,-1.83697019872104E-16));
#7025=DIRECTION('ref_axis',(0.,-1.83697019872104E-16,1.));
#7026=DIRECTION('center_axis',(1.,-3.49148133884313E-15,-1.83697019872104E-16));
#7027=DIRECTION('ref_axis',(1.83697019872103E-16,-1.83697019872104E-16,
1.));
#7028=DIRECTION('center_axis',(3.49148133884313E-15,1.,3.06161699786841E-16));
#7029=DIRECTION('ref_axis',(0.,3.06161699786841E-16,-1.));
#7030=DIRECTION('center_axis',(1.,-3.49148133884313E-15,-1.83697019872104E-16));
#7031=DIRECTION('ref_axis',(1.83697019872103E-16,-1.83697019872104E-16,
1.));
#7032=DIRECTION('center_axis',(-3.71625375700952E-15,-1.,-6.12323399573671E-17));
#7033=DIRECTION('ref_axis',(0.,-1.22464679914734E-16,1.));
#7034=DIRECTION('center_axis',(-1.,3.71625375700953E-15,4.55109826834097E-31));
#7035=DIRECTION('ref_axis',(0.,1.22464679914733E-16,-1.));
#7036=DIRECTION('center_axis',(1.,-3.49148133884313E-15,-1.83697019872104E-16));
#7037=DIRECTION('ref_axis',(1.83697019872103E-16,-1.83697019872103E-16,
1.));
#7038=DIRECTION('center_axis',(1.,-3.49148133884313E-15,-1.83697019872104E-16));
#7039=DIRECTION('ref_axis',(1.83697019872103E-16,-1.83697019872103E-16,
1.));
#7040=DIRECTION('center_axis',(1.,-3.49148133884313E-15,-1.83697019872104E-16));
#7041=DIRECTION('ref_axis',(1.83697019872103E-16,-1.83697019872104E-16,
1.));
#7042=DIRECTION('center_axis',(-1.,3.49148133884313E-15,1.83697019872104E-16));
#7043=DIRECTION('ref_axis',(-1.83697019872103E-16,1.83697019872104E-16,
-1.));
#7044=DIRECTION('center_axis',(0.707106781186544,-0.707106781186551,-3.13590428307428E-16));
#7045=DIRECTION('ref_axis',(0.,-5.14716945902756E-16,1.));
#7046=DIRECTION('center_axis',(0.707106781186544,-0.707106781186551,-3.13590428307428E-16));
#7047=DIRECTION('ref_axis',(-4.73341490577976E-17,-4.90817985800547E-16,
1.));
#7048=DIRECTION('center_axis',(0.707106781186551,0.707106781186544,4.54949803549333E-16));
#7049=DIRECTION('ref_axis',(0.,6.43396182378445E-16,-1.));
#7050=DIRECTION('center_axis',(0.707106781186544,-0.707106781186551,-3.13590428307428E-16));
#7051=DIRECTION('ref_axis',(-4.73341490577977E-17,-4.90817985800548E-16,
1.));
#7052=DIRECTION('center_axis',(-0.707106781186551,-0.707106781186544,-3.05235227668501E-16));
#7053=DIRECTION('ref_axis',(0.,-6.19375626168253E-16,1.));
#7054=DIRECTION('center_axis',(-0.707106781186544,0.707106781186551,2.73727940853274E-16));
#7055=DIRECTION('ref_axis',(0.,3.87109766355158E-16,-1.));
#7056=DIRECTION('center_axis',(0.707106781186544,-0.707106781186551,-3.13590428307428E-16));
#7057=DIRECTION('ref_axis',(-9.1591177670555E-17,-5.35075014413304E-16,
1.));
#7058=DIRECTION('center_axis',(0.707106781186544,-0.707106781186551,-3.13590428307428E-16));
#7059=DIRECTION('ref_axis',(-9.1591177670555E-17,-5.35075014413304E-16,
1.));
#7060=DIRECTION('center_axis',(0.707106781186544,-0.707106781186551,-3.13590428307428E-16));
#7061=DIRECTION('ref_axis',(1.29893408435323E-16,-3.13590428307428E-16,
1.));
#7062=DIRECTION('center_axis',(-0.707106781186544,0.707106781186551,3.13590428307428E-16));
#7063=DIRECTION('ref_axis',(-1.29893408435323E-16,3.13590428307428E-16,
-1.));
#7064=DIRECTION('center_axis',(0.,-1.,-3.67394039744206E-16));
#7065=DIRECTION('ref_axis',(0.,0.,1.));
#7066=DIRECTION('center_axis',(0.,-1.,-3.67394039744206E-16));
#7067=DIRECTION('ref_axis',(0.,-3.67394039744206E-16,1.));
#7068=DIRECTION('center_axis',(1.,-4.49927934798557E-32,1.22464679914735E-16));
#7069=DIRECTION('ref_axis',(1.22464679914735E-16,6.43396182378445E-16,-1.));
#7070=DIRECTION('center_axis',(0.,-1.,-3.67394039744206E-16));
#7071=DIRECTION('ref_axis',(0.,-3.67394039744206E-16,1.));
#7072=DIRECTION('center_axis',(-1.,0.,1.22464679914734E-16));
#7073=DIRECTION('ref_axis',(6.12323399573672E-17,-6.19375626168253E-16,
1.));
#7074=DIRECTION('center_axis',(4.74072736285521E-32,1.,7.74219532710317E-16));
#7075=DIRECTION('ref_axis',(-6.12323399573672E-17,7.74219532710317E-16,
-1.));
#7076=DIRECTION('center_axis',(0.,-1.,-3.67394039744206E-16));
#7077=DIRECTION('ref_axis',(0.,-3.67394039744206E-16,1.));
#7078=DIRECTION('center_axis',(0.,-1.,-3.67394039744206E-16));
#7079=DIRECTION('ref_axis',(0.,-3.67394039744206E-16,1.));
#7080=DIRECTION('center_axis',(0.,-1.,-3.67394039744206E-16));
#7081=DIRECTION('ref_axis',(0.,-3.67394039744206E-16,1.));
#7082=DIRECTION('center_axis',(0.,1.,3.67394039744206E-16));
#7083=DIRECTION('ref_axis',(0.,3.67394039744206E-16,-1.));
#7084=DIRECTION('center_axis',(-0.707106781186554,-0.707106781186541,-3.13590428307426E-16));
#7085=DIRECTION('ref_axis',(0.,-5.14716945902756E-16,1.));
#7086=DIRECTION('center_axis',(-0.707106781186554,-0.707106781186541,-3.13590428307426E-16));
#7087=DIRECTION('ref_axis',(4.73341490577958E-17,-4.9081798580055E-16,1.));
#7088=DIRECTION('center_axis',(0.707106781186541,-0.707106781186554,-2.2747490177467E-16));
#7089=DIRECTION('ref_axis',(0.,3.21698091189223E-16,-1.));
#7090=DIRECTION('center_axis',(-0.707106781186554,-0.707106781186541,-3.13590428307426E-16));
#7091=DIRECTION('ref_axis',(4.73341490577959E-17,-4.9081798580055E-16,1.));
#7092=DIRECTION('center_axis',(-0.707106781186541,0.707106781186554,5.50164587497979E-16));
#7093=DIRECTION('ref_axis',(0.,-6.19375626168253E-16,1.));
#7094=DIRECTION('center_axis',(0.707106781186554,0.707106781186541,2.7372794085327E-16));
#7095=DIRECTION('ref_axis',(0.,3.87109766355158E-16,-1.));
#7096=DIRECTION('center_axis',(-0.707106781186554,-0.707106781186541,-3.13590428307426E-16));
#7097=DIRECTION('ref_axis',(9.15911776705531E-17,-5.35075014413308E-16,
1.));
#7098=DIRECTION('center_axis',(-0.707106781186554,-0.707106781186541,-3.13590428307426E-16));
#7099=DIRECTION('ref_axis',(9.15911776705531E-17,-5.35075014413308E-16,
1.));
#7100=DIRECTION('center_axis',(-0.707106781186554,-0.707106781186541,-3.13590428307426E-16));
#7101=DIRECTION('ref_axis',(-1.29893408435325E-16,-3.13590428307426E-16,
1.));
#7102=DIRECTION('center_axis',(0.707106781186554,0.707106781186541,3.13590428307426E-16));
#7103=DIRECTION('ref_axis',(1.29893408435325E-16,3.13590428307426E-16,-1.));
#7104=DIRECTION('center_axis',(-1.,1.04744440165294E-14,-1.83697019872101E-16));
#7105=DIRECTION('ref_axis',(0.,-1.83697019872098E-16,1.));
#7106=DIRECTION('center_axis',(-1.,1.04744440165294E-14,-1.83697019872101E-16));
#7107=DIRECTION('ref_axis',(-1.83697019872103E-16,-1.83697019872095E-16,
1.));
#7108=DIRECTION('center_axis',(-1.04744440165294E-14,-1.,-6.12323399573585E-17));
#7109=DIRECTION('ref_axis',(0.,6.12323399573585E-17,-1.));
#7110=DIRECTION('center_axis',(-1.,1.04744440165294E-14,-1.83697019872101E-16));
#7111=DIRECTION('ref_axis',(-1.83697019872103E-16,-1.83697019872095E-16,
1.));
#7112=DIRECTION('center_axis',(1.05293856448603E-14,1.,3.06161699786836E-16));
#7113=DIRECTION('ref_axis',(0.,-2.44929359829469E-16,1.));
#7114=DIRECTION('center_axis',(1.,-1.05293856448603E-14,-2.57895568539326E-30));
#7115=DIRECTION('ref_axis',(0.,2.44929359829472E-16,-1.));
#7116=DIRECTION('center_axis',(-1.,1.04744440165294E-14,-1.83697019872101E-16));
#7117=DIRECTION('ref_axis',(-1.83697019872103E-16,-1.83697019872103E-16,
1.));
#7118=DIRECTION('center_axis',(-1.,1.04744440165294E-14,-1.83697019872101E-16));
#7119=DIRECTION('ref_axis',(-1.83697019872103E-16,-1.83697019872103E-16,
1.));
#7120=DIRECTION('center_axis',(-1.,1.04744440165294E-14,-1.83697019872101E-16));
#7121=DIRECTION('ref_axis',(-1.83697019872103E-16,-1.83697019872101E-16,
1.));
#7122=DIRECTION('center_axis',(1.,-1.04744440165294E-14,1.83697019872101E-16));
#7123=DIRECTION('ref_axis',(1.83697019872103E-16,1.83697019872101E-16,-1.));
#7124=DIRECTION('center_axis',(-0.707106781186539,0.707106781186556,-5.38036114367774E-17));
#7125=DIRECTION('ref_axis',(0.,0.,1.));
#7126=DIRECTION('center_axis',(-0.707106781186539,0.707106781186556,-5.38036114367774E-17));
#7127=DIRECTION('ref_axis',(-3.80448984992709E-17,3.80448984992719E-17,
1.));
#7128=DIRECTION('center_axis',(-0.707106781186556,-0.707106781186539,0.));
#7129=DIRECTION('ref_axis',(0.,0.,-1.));
#7130=DIRECTION('center_axis',(-0.707106781186539,0.707106781186556,-5.38036114367774E-17));
#7131=DIRECTION('ref_axis',(-3.80448984992709E-17,3.80448984992719E-17,
1.));
#7132=DIRECTION('center_axis',(0.707106781186556,0.707106781186539,1.22464679914734E-16));
#7133=DIRECTION('ref_axis',(0.,0.,1.));
#7134=DIRECTION('center_axis',(0.707106781186539,-0.707106781186556,0.));
#7135=DIRECTION('ref_axis',(0.,0.,-1.));
#7136=DIRECTION('center_axis',(-0.707106781186539,0.707106781186556,-5.38036114367774E-17));
#7137=DIRECTION('ref_axis',(-3.80448984992709E-17,3.80448984992719E-17,
1.));
#7138=DIRECTION('center_axis',(-0.707106781186539,0.707106781186556,-5.38036114367774E-17));
#7139=DIRECTION('ref_axis',(-3.80448984992709E-17,3.80448984992719E-17,
1.));
#7140=DIRECTION('center_axis',(-0.707106781186539,0.707106781186556,-5.38036114367774E-17));
#7141=DIRECTION('ref_axis',(-1.29893408435322E-16,-5.38036114367772E-17,
1.));
#7142=DIRECTION('center_axis',(0.707106781186539,-0.707106781186556,5.38036114367774E-17));
#7143=DIRECTION('ref_axis',(1.29893408435322E-16,5.38036114367772E-17,-1.));
#7144=DIRECTION('center_axis',(0.,0.,-1.));
#7145=DIRECTION('ref_axis',(-1.,0.,0.));
#7146=DIRECTION('center_axis',(0.,0.,1.));
#7147=DIRECTION('ref_axis',(1.,0.,0.));
#7148=DIRECTION('',(0.,0.,-1.));
#7149=DIRECTION('center_axis',(0.,0.,1.));
#7150=DIRECTION('ref_axis',(1.,0.,0.));
#7151=DIRECTION('center_axis',(0.,0.,-1.));
#7152=DIRECTION('ref_axis',(-1.,0.,0.));
#7153=DIRECTION('center_axis',(0.,0.,1.));
#7154=DIRECTION('ref_axis',(1.,0.,0.));
#7155=DIRECTION('',(0.,0.,1.));
#7156=DIRECTION('center_axis',(0.,0.,1.));
#7157=DIRECTION('ref_axis',(1.,0.,0.));
#7158=DIRECTION('center_axis',(0.,0.,1.));
#7159=DIRECTION('ref_axis',(1.,0.,0.));
#7160=DIRECTION('center_axis',(0.,0.,1.));
#7161=DIRECTION('ref_axis',(1.,0.,0.));
#7162=DIRECTION('center_axis',(0.,1.83697019872103E-16,-1.));
#7163=DIRECTION('ref_axis',(0.,1.,1.5654552317848E-16));
#7164=DIRECTION('center_axis',(0.,1.83697019872103E-16,-1.));
#7165=DIRECTION('ref_axis',(0.,1.,1.83697019872103E-16));
#7166=DIRECTION('center_axis',(-1.,1.22464679914735E-16,2.24963967399279E-32));
#7167=DIRECTION('ref_axis',(-1.22464679914735E-16,-1.,-1.956819039731E-16));
#7168=DIRECTION('center_axis',(0.,-1.83697019872103E-16,1.));
#7169=DIRECTION('ref_axis',(0.,1.,1.83697019872103E-16));
#7170=DIRECTION('center_axis',(0.,-1.83697019872103E-16,1.));
#7171=DIRECTION('ref_axis',(0.,1.,1.83697019872103E-16));
#7172=DIRECTION('center_axis',(0.,1.83697019872103E-16,-1.));
#7173=DIRECTION('ref_axis',(0.,1.,1.93432686686053E-16));
#7174=DIRECTION('center_axis',(0.,1.83697019872103E-16,-1.));
#7175=DIRECTION('ref_axis',(0.,1.,1.83697019872103E-16));
#7176=DIRECTION('center_axis',(0.,1.83697019872103E-16,-1.));
#7177=DIRECTION('ref_axis',(0.,1.,1.83697019872103E-16));
#7178=DIRECTION('center_axis',(-1.,1.22464679914735E-16,2.24963967399279E-32));
#7179=DIRECTION('ref_axis',(-1.22464679914735E-16,-1.,-1.6119390557171E-16));
#7180=DIRECTION('center_axis',(0.,-1.83697019872103E-16,1.));
#7181=DIRECTION('ref_axis',(0.,1.,1.83697019872103E-16));
#7182=DIRECTION('center_axis',(0.,-1.83697019872103E-16,1.));
#7183=DIRECTION('ref_axis',(0.,-1.,-1.83697019872103E-16));
#7184=DIRECTION('',(0.,1.83697019872103E-16,-1.));
#7185=DIRECTION('center_axis',(0.,-1.83697019872103E-16,1.));
#7186=DIRECTION('ref_axis',(0.,-1.,-1.83697019872103E-16));
#7187=DIRECTION('center_axis',(0.,-1.83697019872103E-16,1.));
#7188=DIRECTION('ref_axis',(0.,-1.,-1.83697019872103E-16));
#7189=DIRECTION('center_axis',(0.,1.83697019872103E-16,-1.));
#7190=DIRECTION('ref_axis',(0.,1.,1.83697019872103E-16));
#7191=DIRECTION('center_axis',(0.,-1.83697019872103E-16,1.));
#7192=DIRECTION('ref_axis',(0.,-1.,-1.83697019872103E-16));
#7193=DIRECTION('',(9.0785384304179E-17,0.741318920421686,0.671152932069007));
#7194=DIRECTION('center_axis',(0.,-1.83697019872103E-16,1.));
#7195=DIRECTION('ref_axis',(0.,-1.,-1.83697019872103E-16));
#7196=DIRECTION('center_axis',(0.,-1.83697019872103E-16,1.));
#7197=DIRECTION('ref_axis',(0.,-1.,-1.83697019872103E-16));
#7198=DIRECTION('',(-9.07853843041783E-17,0.741318920421681,0.671152932069013));
#7199=DIRECTION('center_axis',(0.,-1.83697019872103E-16,1.));
#7200=DIRECTION('ref_axis',(0.,-1.,-1.83697019872103E-16));
#7201=DIRECTION('center_axis',(0.,-1.83697019872103E-16,1.));
#7202=DIRECTION('ref_axis',(0.,-1.,-1.83697019872103E-16));
#7203=DIRECTION('',(0.,-1.83697019872103E-16,1.));
#7204=DIRECTION('center_axis',(0.,1.83697019872103E-16,-1.));
#7205=DIRECTION('ref_axis',(0.,1.,1.83697019872103E-16));
#7206=DIRECTION('center_axis',(0.,-1.83697019872103E-16,1.));
#7207=DIRECTION('ref_axis',(0.,-1.,-1.83697019872103E-16));
#7208=DIRECTION('center_axis',(0.,-1.83697019872103E-16,1.));
#7209=DIRECTION('ref_axis',(0.,-1.,-1.93432686686053E-16));
#7210=DIRECTION('center_axis',(0.,-1.83697019872103E-16,1.));
#7211=DIRECTION('ref_axis',(0.,-1.,-1.83697019872103E-16));
#7212=DIRECTION('center_axis',(-1.,-1.22464679914735E-16,-2.24963967399279E-32));
#7213=DIRECTION('ref_axis',(-1.22464679914735E-16,1.,1.6119390557171E-16));
#7214=DIRECTION('center_axis',(0.,1.83697019872103E-16,-1.));
#7215=DIRECTION('ref_axis',(0.,-1.,-1.83697019872103E-16));
#7216=DIRECTION('center_axis',(0.,-1.83697019872103E-16,1.));
#7217=DIRECTION('ref_axis',(0.,-1.,-1.5654552317848E-16));
#7218=DIRECTION('center_axis',(0.,-1.83697019872103E-16,1.));
#7219=DIRECTION('ref_axis',(0.,-1.,-1.83697019872103E-16));
#7220=DIRECTION('center_axis',(-1.,-1.22464679914735E-16,-2.24963967399279E-32));
#7221=DIRECTION('ref_axis',(-1.22464679914735E-16,1.,1.956819039731E-16));
#7222=DIRECTION('center_axis',(0.,1.83697019872103E-16,-1.));
#7223=DIRECTION('ref_axis',(0.,-1.,-1.83697019872103E-16));
#7224=DIRECTION('center_axis',(0.,-1.83697019872103E-16,1.));
#7225=DIRECTION('ref_axis',(0.,-1.,-1.83697019872103E-16));
#7226=DIRECTION('',(0.,-1.83697019872103E-16,1.));
#7227=DIRECTION('center_axis',(0.,-1.83697019872103E-16,1.));
#7228=DIRECTION('ref_axis',(0.,-1.,-1.83697019872103E-16));
#7229=DIRECTION('center_axis',(0.,-1.83697019872103E-16,1.));
#7230=DIRECTION('ref_axis',(0.,-1.,-1.83697019872103E-16));
#7231=DIRECTION('center_axis',(0.,1.83697019872103E-16,-1.));
#7232=DIRECTION('ref_axis',(0.,1.,1.83697019872103E-16));
#7233=DIRECTION('center_axis',(0.,-1.83697019872103E-16,1.));
#7234=DIRECTION('ref_axis',(0.,-1.,-1.83697019872103E-16));
#7235=DIRECTION('',(-9.07853843041785E-17,-0.741318920421682,-0.671152932069012));
#7236=DIRECTION('center_axis',(0.,-1.83697019872103E-16,1.));
#7237=DIRECTION('ref_axis',(0.,-1.,-1.83697019872103E-16));
#7238=DIRECTION('center_axis',(0.,-1.83697019872103E-16,1.));
#7239=DIRECTION('ref_axis',(0.,-1.,-1.83697019872103E-16));
#7240=DIRECTION('',(9.07853843041792E-17,-0.741318920421688,-0.671152932069005));
#7241=DIRECTION('center_axis',(0.,-1.83697019872103E-16,1.));
#7242=DIRECTION('ref_axis',(0.,-1.,-1.83697019872103E-16));
#7243=DIRECTION('center_axis',(0.,-1.83697019872103E-16,1.));
#7244=DIRECTION('ref_axis',(0.,-1.,-1.83697019872103E-16));
#7245=DIRECTION('',(0.,1.83697019872103E-16,-1.));
#7246=DIRECTION('center_axis',(0.,1.83697019872103E-16,-1.));
#7247=DIRECTION('ref_axis',(0.,1.,1.83697019872103E-16));
#7248=DIRECTION('center_axis',(0.,-1.83697019872103E-16,1.));
#7249=DIRECTION('ref_axis',(0.,-1.,-1.83697019872103E-16));
#7250=DIRECTION('axis',(0.,0.,1.));
#7251=DIRECTION('refdir',(1.,0.,0.));
#7252=DIRECTION('center_axis',(0.,0.,-1.));
#7253=DIRECTION('ref_axis',(-1.,0.,0.));
#7254=DIRECTION('center_axis',(0.,0.,-1.));
#7255=DIRECTION('ref_axis',(-1.,0.,0.));
#7256=DIRECTION('',(0.,0.,-1.));
#7257=DIRECTION('center_axis',(0.,0.,-1.));
#7258=DIRECTION('ref_axis',(-1.,0.,0.));
#7259=DIRECTION('',(0.,0.,-1.));
#7260=DIRECTION('center_axis',(0.,0.,1.));
#7261=DIRECTION('ref_axis',(-1.,0.,0.));
#7262=DIRECTION('center_axis',(0.,0.,-1.));
#7263=DIRECTION('ref_axis',(-1.,0.,0.));
#7264=DIRECTION('center_axis',(0.,0.,-1.));
#7265=DIRECTION('ref_axis',(-1.,0.,0.));
#7266=DIRECTION('',(0.,0.,-1.));
#7267=DIRECTION('center_axis',(0.,0.,-1.));
#7268=DIRECTION('ref_axis',(-1.,0.,0.));
#7269=DIRECTION('',(0.,0.,-1.));
#7270=DIRECTION('center_axis',(0.,0.,1.));
#7271=DIRECTION('ref_axis',(-1.,0.,0.));
#7272=DIRECTION('center_axis',(0.,0.,-1.));
#7273=DIRECTION('ref_axis',(-1.,0.,0.));
#7274=DIRECTION('center_axis',(0.,0.,-1.));
#7275=DIRECTION('ref_axis',(-1.,0.,0.));
#7276=DIRECTION('',(0.,0.,-1.));
#7277=DIRECTION('center_axis',(0.,0.,-1.));
#7278=DIRECTION('ref_axis',(-1.,0.,0.));
#7279=DIRECTION('',(0.,0.,-1.));
#7280=DIRECTION('center_axis',(0.,0.,1.));
#7281=DIRECTION('ref_axis',(-1.,0.,0.));
#7282=DIRECTION('center_axis',(0.,0.,-1.));
#7283=DIRECTION('ref_axis',(-1.,0.,0.));
#7284=DIRECTION('center_axis',(0.,0.,-1.));
#7285=DIRECTION('ref_axis',(-1.,0.,0.));
#7286=DIRECTION('',(0.,0.,-1.));
#7287=DIRECTION('center_axis',(0.,0.,-1.));
#7288=DIRECTION('ref_axis',(-1.,0.,0.));
#7289=DIRECTION('',(0.,0.,-1.));
#7290=DIRECTION('center_axis',(0.,0.,1.));
#7291=DIRECTION('ref_axis',(-1.,0.,0.));
#7292=DIRECTION('center_axis',(0.,-0.707106781186547,0.707106781186548));
#7293=DIRECTION('ref_axis',(0.,-0.707106781186548,-0.707106781186547));
#7294=DIRECTION('',(0.,-0.707106781186548,-0.707106781186547));
#7295=DIRECTION('',(1.,0.,0.));
#7296=DIRECTION('',(0.,0.707106781186548,0.707106781186547));
#7297=DIRECTION('',(1.,0.,0.));
#7298=DIRECTION('center_axis',(0.,0.,1.));
#7299=DIRECTION('ref_axis',(0.,-1.,0.));
#7300=DIRECTION('',(0.,-1.,0.));
#7301=DIRECTION('',(1.,0.,0.));
#7302=DIRECTION('',(0.,1.,0.));
#7303=DIRECTION('center_axis',(0.,0.707106781186548,0.707106781186548));
#7304=DIRECTION('ref_axis',(0.,-0.707106781186548,0.707106781186548));
#7305=DIRECTION('',(0.,-0.707106781186547,0.707106781186547));
#7306=DIRECTION('',(-1.,0.,0.));
#7307=DIRECTION('',(0.,0.707106781186547,-0.707106781186547));
#7308=DIRECTION('center_axis',(0.,0.,-1.));
#7309=DIRECTION('ref_axis',(-1.,0.,0.));
#7310=DIRECTION('',(0.,-1.,0.));
#7311=DIRECTION('',(1.,0.,0.));
#7312=DIRECTION('',(0.,1.,0.));
#7313=DIRECTION('center_axis',(0.,0.,-1.));
#7314=DIRECTION('ref_axis',(-1.,0.,0.));
#7315=DIRECTION('',(0.,1.,0.));
#7316=DIRECTION('',(1.,0.,0.));
#7317=DIRECTION('',(0.,-1.,0.));
#7318=DIRECTION('center_axis',(-1.,0.,0.));
#7319=DIRECTION('ref_axis',(0.,-1.,0.));
#7320=DIRECTION('',(0.,0.707106781186547,-0.707106781186548));
#7321=DIRECTION('',(0.,0.,1.));
#7322=DIRECTION('',(0.,-0.707106781186547,-0.707106781186548));
#7323=DIRECTION('',(0.,-1.,0.));
#7324=DIRECTION('',(0.,0.707106781186548,-0.707106781186547));
#7325=DIRECTION('',(0.,1.,0.));
#7326=DIRECTION('',(0.,0.707106781186547,0.707106781186547));
#7327=DIRECTION('',(0.,-1.,0.));
#7328=DIRECTION('',(0.,0.707106781186547,-0.707106781186547));
#7329=DIRECTION('',(0.,1.,0.));
#7330=DIRECTION('',(0.,0.707106781186548,0.707106781186547));
#7331=DIRECTION('',(0.,-1.,0.));
#7332=DIRECTION('',(0.,-0.707106781186547,0.707106781186548));
#7333=DIRECTION('',(0.,0.,1.));
#7334=DIRECTION('',(0.,0.707106781186547,0.707106781186548));
#7335=DIRECTION('',(0.,1.,0.));
#7336=DIRECTION('',(0.,-0.707106781186548,0.707106781186547));
#7337=DIRECTION('',(0.,-1.,0.));
#7338=DIRECTION('',(0.,-0.707106781186547,-0.707106781186547));
#7339=DIRECTION('center_axis',(1.,0.,0.));
#7340=DIRECTION('ref_axis',(0.,-1.,0.));
#7341=DIRECTION('center_axis',(1.,0.,0.));
#7342=DIRECTION('ref_axis',(0.,1.,0.));
#7343=DIRECTION('center_axis',(1.,0.,0.));
#7344=DIRECTION('ref_axis',(0.,1.,0.));
#7345=DIRECTION('center_axis',(0.,-0.707106781186547,-0.707106781186548));
#7346=DIRECTION('ref_axis',(0.,0.707106781186548,-0.707106781186547));
#7347=DIRECTION('',(-1.,0.,0.));
#7348=DIRECTION('',(0.,0.707106781186548,-0.707106781186547));
#7349=DIRECTION('',(1.,0.,0.));
#7350=DIRECTION('center_axis',(0.,0.,-1.));
#7351=DIRECTION('ref_axis',(0.,1.,0.));
#7352=DIRECTION('',(0.,1.,0.));
#7353=DIRECTION('',(1.,0.,0.));
#7354=DIRECTION('center_axis',(0.,0.707106781186548,-0.707106781186548));
#7355=DIRECTION('ref_axis',(0.,0.707106781186548,0.707106781186548));
#7356=DIRECTION('',(0.,0.707106781186547,0.707106781186547));
#7357=DIRECTION('center_axis',(1.,0.,0.));
#7358=DIRECTION('ref_axis',(0.,1.,0.));
#7359=DIRECTION('',(0.,-1.,0.));
#7360=DIRECTION('',(0.,-0.707106781186547,-0.707106781186548));
#7361=DIRECTION('',(0.,0.,-1.));
#7362=DIRECTION('',(0.,0.707106781186547,-0.707106781186548));
#7363=DIRECTION('',(0.,1.,0.));
#7364=DIRECTION('',(0.,-0.707106781186548,-0.707106781186547));
#7365=DIRECTION('',(0.,-1.,0.));
#7366=DIRECTION('',(0.,-0.707106781186547,0.707106781186547));
#7367=DIRECTION('',(0.,1.,0.));
#7368=DIRECTION('',(0.,-0.707106781186547,-0.707106781186547));
#7369=DIRECTION('',(0.,-1.,0.));
#7370=DIRECTION('',(0.,-0.707106781186548,0.707106781186547));
#7371=DIRECTION('',(0.,1.,0.));
#7372=DIRECTION('',(0.,0.707106781186547,0.707106781186548));
#7373=DIRECTION('',(0.,0.,1.));
#7374=DIRECTION('',(0.,-0.707106781186547,0.707106781186548));
#7375=DIRECTION('center_axis',(-1.,0.,0.));
#7376=DIRECTION('ref_axis',(0.,-1.,0.));
#7377=DIRECTION('center_axis',(-1.,0.,0.));
#7378=DIRECTION('ref_axis',(0.,1.,0.));
#7379=DIRECTION('center_axis',(-1.,0.,0.));
#7380=DIRECTION('ref_axis',(0.,1.,0.));
#7381=DIRECTION('center_axis',(0.,0.,-1.));
#7382=DIRECTION('ref_axis',(-1.,0.,0.));
#7383=DIRECTION('',(-1.,0.,0.));
#7384=DIRECTION('center_axis',(0.,0.707106781186547,0.707106781186548));
#7385=DIRECTION('ref_axis',(0.,-0.707106781186548,0.707106781186547));
#7386=DIRECTION('',(-1.,0.,0.));
#7387=DIRECTION('',(1.,0.,0.));
#7388=DIRECTION('center_axis',(0.,0.,1.));
#7389=DIRECTION('ref_axis',(0.,-1.,0.));
#7390=DIRECTION('',(1.,0.,0.));
#7391=DIRECTION('center_axis',(0.,-0.707106781186548,0.707106781186548));
#7392=DIRECTION('ref_axis',(0.,-0.707106781186548,-0.707106781186548));
#7393=DIRECTION('',(1.,0.,0.));
#7394=DIRECTION('center_axis',(0.,0.,1.));
#7395=DIRECTION('ref_axis',(1.,0.,0.));
#7396=DIRECTION('',(-1.,0.,0.));
#7397=DIRECTION('center_axis',(0.,0.,1.));
#7398=DIRECTION('ref_axis',(1.,0.,0.));
#7399=DIRECTION('',(-1.,0.,0.));
#7400=DIRECTION('center_axis',(0.,0.707106781186547,-0.707106781186548));
#7401=DIRECTION('ref_axis',(0.,0.707106781186548,0.707106781186547));
#7402=DIRECTION('',(1.,0.,0.));
#7403=DIRECTION('',(1.,0.,0.));
#7404=DIRECTION('center_axis',(0.,0.,-1.));
#7405=DIRECTION('ref_axis',(0.,1.,0.));
#7406=DIRECTION('',(1.,0.,0.));
#7407=DIRECTION('center_axis',(0.,-0.707106781186548,-0.707106781186548));
#7408=DIRECTION('ref_axis',(0.,0.707106781186548,-0.707106781186548));
#7409=DIRECTION('center_axis',(0.,0.,1.));
#7410=DIRECTION('ref_axis',(1.,0.,0.));
#7411=DIRECTION('',(1.,0.,0.));
#7412=DIRECTION('center_axis',(1.,0.,0.));
#7413=DIRECTION('ref_axis',(0.,-1.,0.));
#7414=DIRECTION('',(1.,0.,0.));
#7415=DIRECTION('center_axis',(-1.,0.,0.));
#7416=DIRECTION('ref_axis',(0.,1.,0.));
#7417=DIRECTION('',(-1.,0.,0.));
#7418=DIRECTION('center_axis',(-1.,0.,0.));
#7419=DIRECTION('ref_axis',(0.,1.,0.));
#7420=DIRECTION('',(-1.,0.,0.));
#7421=DIRECTION('center_axis',(0.,0.707106781186548,-0.707106781186547));
#7422=DIRECTION('ref_axis',(-1.,0.,0.));
#7423=DIRECTION('',(1.,0.,0.));
#7424=DIRECTION('center_axis',(0.,1.,0.));
#7425=DIRECTION('ref_axis',(-1.,0.,0.));
#7426=DIRECTION('',(-1.,0.,0.));
#7427=DIRECTION('center_axis',(0.,0.707106781186548,0.707106781186547));
#7428=DIRECTION('ref_axis',(1.,0.,0.));
#7429=DIRECTION('center_axis',(0.,-0.707106781186548,-0.707106781186547));
#7430=DIRECTION('ref_axis',(-1.,0.,0.));
#7431=DIRECTION('',(-1.,0.,0.));
#7432=DIRECTION('center_axis',(0.,-1.,0.));
#7433=DIRECTION('ref_axis',(1.,0.,0.));
#7434=DIRECTION('',(1.,0.,0.));
#7435=DIRECTION('center_axis',(0.,-0.707106781186548,0.707106781186547));
#7436=DIRECTION('ref_axis',(1.,0.,0.));
#7437=DIRECTION('',(1.,-8.32667268468867E-17,-2.95822839457879E-31));
#7438=DIRECTION('',(3.45434621840759E-16,1.73708262759656E-16,-1.));
#7439=DIRECTION('',(-1.,1.22464679914735E-16,0.));
#7440=DIRECTION('',(0.,0.,1.));
#7441=DIRECTION('',(-3.54369311672542E-14,-1.,5.55111512312579E-17));
#7442=DIRECTION('',(3.47046641137479E-18,5.55111512312578E-17,1.));
#7443=DIRECTION('',(0.,0.,1.));
#7444=DIRECTION('',(1.,0.,0.));
#7445=DIRECTION('',(0.,0.,1.));
#7446=DIRECTION('',(1.,0.,0.));
#7447=DIRECTION('',(-1.,-2.7755575615629E-17,2.95822839457879E-31));
#7448=DIRECTION('',(2.95822839457879E-31,2.77555756156287E-17,1.));
#7449=DIRECTION('',(-1.,6.98660572945338E-169,2.95822839457879E-31));
#7450=DIRECTION('',(-2.95822839457879E-31,-5.55111512312574E-17,-1.));
#7451=DIRECTION('',(1.,4.47500443872012E-154,-2.9582283945788E-31));
#7452=DIRECTION('',(-1.21700038808115E-17,-7.7570958372768E-16,0.999999999999999));
#7453=DIRECTION('',(-1.,0.,0.));
#7454=DIRECTION('',(0.,0.,-1.));
#7455=DIRECTION('',(1.,0.,0.));
#7456=DIRECTION('',(0.,0.,-1.));
#7457=DIRECTION('',(1.,0.,0.));
#7458=DIRECTION('',(0.,0.,1.));
#7459=DIRECTION('',(0.,0.,1.));
#7460=DIRECTION('',(1.,0.,0.));
#7461=DIRECTION('',(0.,0.,1.));
#7462=DIRECTION('',(1.,0.,0.));
#7463=DIRECTION('',(0.,0.,1.));
#7464=DIRECTION('',(1.,0.,0.));
#7465=DIRECTION('',(1.,5.55111512312581E-17,-2.9582283945788E-31));
#7466=DIRECTION('',(6.37054347935888E-17,3.13421272546651E-16,-0.999999999999999));
#7467=DIRECTION('',(1.,1.16573417585641E-15,-2.9582283945788E-31));
#7468=DIRECTION('',(3.84911901736414E-17,1.73011627517047E-16,-1.));
#7469=DIRECTION('',(2.95822839457879E-31,-2.4980018054066E-16,1.));
#7470=DIRECTION('',(1.,-2.42892240612031E-77,-2.9582283945788E-31));
#7471=CARTESIAN_POINT('',(0.,0.,0.));
#7472=CARTESIAN_POINT('',(0.,0.,0.));
#7473=CARTESIAN_POINT('Origin',(140.,37.8343839603864,-8.00000000000001));
#7474=CARTESIAN_POINT('',(-130.,31.8343839603864,-8.00000000000001));
#7475=CARTESIAN_POINT('Origin',(-130.,37.8343839603864,-8.00000000000001));
#7476=CARTESIAN_POINT('',(-145.,31.8343839603864,-8.00000000000001));
#7477=CARTESIAN_POINT('',(140.,31.8343839603864,-8.00000000000001));
#7478=CARTESIAN_POINT('Origin',(-145.,37.8343839603864,-8.00000000000001));
#7479=CARTESIAN_POINT('Origin',(-145.,37.8343839603864,-8.00000000000001));
#7480=CARTESIAN_POINT('',(-145.,32.8343839603866,-8.00000000000001));
#7481=CARTESIAN_POINT('Origin',(-145.,37.8343839603864,-8.00000000000001));
#7482=CARTESIAN_POINT('Origin',(-140.,-23.6740181268338,20.));
#7483=CARTESIAN_POINT('',(-144.,-23.6740181268338,20.));
#7484=CARTESIAN_POINT('Origin',(-140.,-23.6740181268338,20.));
#7485=CARTESIAN_POINT('',(-144.,-23.6740181268338,0.));
#7486=CARTESIAN_POINT('',(-144.,-23.6740181268338,20.));
#7487=CARTESIAN_POINT('Origin',(-140.,-23.6740181268338,0.));
#7488=CARTESIAN_POINT('Origin',(-140.,-23.6740181268338,0.));
#7489=CARTESIAN_POINT('Origin',(-140.,23.6740181268338,20.));
#7490=CARTESIAN_POINT('',(-144.,23.6740181268338,20.));
#7491=CARTESIAN_POINT('Origin',(-140.,23.6740181268338,20.));
#7492=CARTESIAN_POINT('',(-144.,23.6740181268338,0.));
#7493=CARTESIAN_POINT('',(-144.,23.6740181268338,20.));
#7494=CARTESIAN_POINT('Origin',(-140.,23.6740181268338,0.));
#7495=CARTESIAN_POINT('Origin',(-140.,23.6740181268338,0.));
#7496=CARTESIAN_POINT('Origin',(-140.,-50.,8.77546295170414));
#7497=CARTESIAN_POINT('',(-145.,-50.,8.77546295170414));
#7498=CARTESIAN_POINT('Origin',(-140.,-50.,8.77546295170414));
#7499=CARTESIAN_POINT('',(-145.,-42.,8.77546295170414));
#7500=CARTESIAN_POINT('',(-145.,-50.,8.77546295170414));
#7501=CARTESIAN_POINT('Origin',(-140.,-42.,8.77546295170414));
#7502=CARTESIAN_POINT('Origin',(-140.,-42.,8.77546295170414));
#7503=CARTESIAN_POINT('',(-143.,-42.,8.77546295170414));
#7504=CARTESIAN_POINT('Origin',(-140.,-42.,8.77546295170414));
#7505=CARTESIAN_POINT('Origin',(-140.,-50.,8.77546295170414));
#7506=CARTESIAN_POINT('',(-143.,-38.3343839603864,8.77546295170414));
#7507=CARTESIAN_POINT('',(-143.,-50.,8.77546295170414));
#7508=CARTESIAN_POINT('Origin',(-140.,-38.3343839603864,8.77546295170414));
#7509=CARTESIAN_POINT('Origin',(-140.,-50.,8.77546295170414));
#7510=CARTESIAN_POINT('',(-143.,-37.3343839603864,8.77546295170414));
#7511=CARTESIAN_POINT('Origin',(-140.,-37.3343839603864,8.77546295170414));
#7512=CARTESIAN_POINT('',(-143.,-30.,8.77546295170414));
#7513=CARTESIAN_POINT('',(-143.,-50.,8.77546295170414));
#7514=CARTESIAN_POINT('Origin',(-140.,-30.,8.77546295170414));
#7515=CARTESIAN_POINT('Origin',(-140.,-30.,8.77546295170414));
#7516=CARTESIAN_POINT('Origin',(-150.,37.8343839603864,-8.00000000000001));
#7517=CARTESIAN_POINT('',(-150.,32.8343839603866,-8.00000000000001));
#7518=CARTESIAN_POINT('',(-150.,32.8343839603866,-8.00000000000001));
#7519=CARTESIAN_POINT('Origin',(-150.,37.8343839603864,-8.00000000000001));
#7520=CARTESIAN_POINT('Origin',(-150.,-37.8343839603864,-8.00000000000001));
#7521=CARTESIAN_POINT('',(-140.,-38.3343839603864,-3.02506281446715));
#7522=CARTESIAN_POINT('',(-150.,-38.3343839603864,-3.02506281446715));
#7523=CARTESIAN_POINT('',(-150.,-38.3343839603864,-3.02506281446715));
#7524=CARTESIAN_POINT('',(-140.,-37.3343839603864,-3.02506281446715));
#7525=CARTESIAN_POINT('Origin',(-140.,-37.8343839603864,-8.00000000000001));
#7526=CARTESIAN_POINT('',(-150.,-37.3343839603864,-3.02506281446715));
#7527=CARTESIAN_POINT('',(-150.,-37.3343839603864,-3.02506281446715));
#7528=CARTESIAN_POINT('Origin',(-150.,-37.8343839603864,-8.00000000000001));
#7529=CARTESIAN_POINT('Origin',(-150.,50.,0.));
#7530=CARTESIAN_POINT('',(-150.,-37.3343839603864,19.));
#7531=CARTESIAN_POINT('',(-150.,-37.3343839603864,10.));
#7532=CARTESIAN_POINT('',(-150.,49.,19.));
#7533=CARTESIAN_POINT('',(-150.,25.,19.));
#7534=CARTESIAN_POINT('',(-150.,49.,-19.));
#7535=CARTESIAN_POINT('',(-150.,49.,0.));
#7536=CARTESIAN_POINT('',(-150.,-49.,-19.));
#7537=CARTESIAN_POINT('',(-150.,25.,-19.));
#7538=CARTESIAN_POINT('',(-150.,-49.,19.));
#7539=CARTESIAN_POINT('',(-150.,-49.,0.));
#7540=CARTESIAN_POINT('',(-150.,-38.3343839603864,19.));
#7541=CARTESIAN_POINT('',(-150.,25.,19.));
#7542=CARTESIAN_POINT('',(-150.,-38.3343839603864,10.));
#7543=CARTESIAN_POINT('Origin',(-155.071229108474,-37.3343839603864,20.));
#7544=CARTESIAN_POINT('',(-140.,-37.3343839603864,-2.02086962844929));
#7545=CARTESIAN_POINT('',(-140.,-37.3343839603864,6.));
#7546=CARTESIAN_POINT('',(-130.,-37.3343839603864,-2.02086962844929));
#7547=CARTESIAN_POINT('',(0.,-37.3343839603864,-2.02086962844929));
#7548=CARTESIAN_POINT('',(-130.,-37.3343839603864,19.));
#7549=CARTESIAN_POINT('',(-130.,-37.3343839603864,10.));
#7550=CARTESIAN_POINT('',(-131.,-37.3343839603864,20.));
#7551=CARTESIAN_POINT('Origin',(-131.,-37.3343839603864,19.));
#7552=CARTESIAN_POINT('',(-149.,-37.3343839603864,20.));
#7553=CARTESIAN_POINT('',(-147.535614554237,-37.3343839603864,20.));
#7554=CARTESIAN_POINT('Origin',(-149.,-37.3343839603864,19.));
#7555=CARTESIAN_POINT('Origin',(-140.,-37.8343839603864,-7.99999999999999));
#7556=CARTESIAN_POINT('',(-140.,-38.3343839603864,-2.02086962844929));
#7557=CARTESIAN_POINT('',(-140.,-38.3343839603864,6.));
#7558=CARTESIAN_POINT('Origin',(-140.,-37.8343839603864,-7.99999999999999));
#7559=CARTESIAN_POINT('Origin',(-124.928770891526,-38.3343839603864,20.));
#7560=CARTESIAN_POINT('',(-149.,-38.3343839603864,20.));
#7561=CARTESIAN_POINT('Origin',(-149.,-38.3343839603864,19.));
#7562=CARTESIAN_POINT('',(-131.,-38.3343839603864,20.));
#7563=CARTESIAN_POINT('',(-132.464385445763,-38.3343839603864,20.));
#7564=CARTESIAN_POINT('',(-130.,-38.3343839603864,19.));
#7565=CARTESIAN_POINT('Origin',(-131.,-38.3343839603864,19.));
#7566=CARTESIAN_POINT('',(-130.,-38.3343839603864,-2.02086962844929));
#7567=CARTESIAN_POINT('',(-130.,-38.3343839603864,10.));
#7568=CARTESIAN_POINT('',(0.,-38.3343839603864,-2.02086962844929));
#7569=CARTESIAN_POINT('Origin',(-149.,25.,19.));
#7570=CARTESIAN_POINT('',(-149.,49.,20.));
#7571=CARTESIAN_POINT('',(-149.,25.,20.));
#7572=CARTESIAN_POINT('Origin',(-149.,49.,19.));
#7573=CARTESIAN_POINT('Origin',(-140.,8.88178419700125E-15,20.));
#7574=CARTESIAN_POINT('',(-131.,49.,20.));
#7575=CARTESIAN_POINT('',(-131.,-25.,20.));
#7576=CARTESIAN_POINT('',(-135.,49.,20.));
#7577=CARTESIAN_POINT('Origin',(-131.,-25.,19.));
#7578=CARTESIAN_POINT('',(-130.,49.,19.));
#7579=CARTESIAN_POINT('',(-130.,-25.,19.));
#7580=CARTESIAN_POINT('Origin',(-131.,49.,19.));
#7581=CARTESIAN_POINT('Origin',(-131.,-25.,19.));
#7582=CARTESIAN_POINT('',(-131.,-49.,20.));
#7583=CARTESIAN_POINT('',(-131.,-25.,20.));
#7584=CARTESIAN_POINT('',(-130.,-49.,19.));
#7585=CARTESIAN_POINT('Origin',(-131.,-49.,19.));
#7586=CARTESIAN_POINT('',(-130.,-25.,19.));
#7587=CARTESIAN_POINT('Origin',(-131.,-49.,-19.));
#7588=CARTESIAN_POINT('',(-130.,-49.,-19.));
#7589=CARTESIAN_POINT('',(-131.,-49.,-20.));
#7590=CARTESIAN_POINT('Origin',(-131.,-49.,-19.));
#7591=CARTESIAN_POINT('',(-131.,-50.,-19.));
#7592=CARTESIAN_POINT('Origin',(-131.,-49.,-19.));
#7593=CARTESIAN_POINT('Origin',(-131.,-49.,-19.));
#7594=CARTESIAN_POINT('Origin',(-131.,-49.,19.));
#7595=CARTESIAN_POINT('',(-131.,-50.,19.));
#7596=CARTESIAN_POINT('Origin',(-131.,-49.,19.));
#7597=CARTESIAN_POINT('Origin',(-131.,-49.,19.));
#7598=CARTESIAN_POINT('Origin',(-131.,-49.,0.));
#7599=CARTESIAN_POINT('',(-131.,-50.,0.));
#7600=CARTESIAN_POINT('',(-130.,-49.,0.));
#7601=CARTESIAN_POINT('Origin',(-149.,-49.,-19.));
#7602=CARTESIAN_POINT('',(-149.,-50.,-19.));
#7603=CARTESIAN_POINT('',(-149.,-49.,-20.));
#7604=CARTESIAN_POINT('Origin',(-149.,-49.,-19.));
#7605=CARTESIAN_POINT('Origin',(-149.,-49.,-19.));
#7606=CARTESIAN_POINT('Origin',(-149.,-49.,-19.));
#7607=CARTESIAN_POINT('Origin',(-131.,49.,19.));
#7608=CARTESIAN_POINT('',(-131.,50.,19.));
#7609=CARTESIAN_POINT('Origin',(-131.,49.,19.));
#7610=CARTESIAN_POINT('Origin',(-131.,49.,19.));
#7611=CARTESIAN_POINT('Origin',(-131.,49.,0.));
#7612=CARTESIAN_POINT('',(-131.,50.,-20.));
#7613=CARTESIAN_POINT('',(-131.,50.,0.));
#7614=CARTESIAN_POINT('',(-130.,49.,-19.));
#7615=CARTESIAN_POINT('',(-130.,49.,0.));
#7616=CARTESIAN_POINT('Origin',(-131.,49.,-19.));
#7617=CARTESIAN_POINT('Origin',(-149.,-49.,19.));
#7618=CARTESIAN_POINT('',(-149.,-49.,20.));
#7619=CARTESIAN_POINT('Origin',(-149.,-49.,19.));
#7620=CARTESIAN_POINT('',(-149.,-50.,19.));
#7621=CARTESIAN_POINT('Origin',(-149.,-49.,19.));
#7622=CARTESIAN_POINT('Origin',(-149.,-49.,19.));
#7623=CARTESIAN_POINT('Origin',(-149.,-49.,0.));
#7624=CARTESIAN_POINT('',(-149.,-50.,0.));
#7625=CARTESIAN_POINT('Origin',(-145.,-49.,19.));
#7626=CARTESIAN_POINT('',(-145.,-49.,20.));
#7627=CARTESIAN_POINT('',(-145.,-50.,19.));
#7628=CARTESIAN_POINT('Origin',(-149.,49.,19.));
#7629=CARTESIAN_POINT('',(-149.,50.,19.));
#7630=CARTESIAN_POINT('Origin',(-149.,49.,19.));
#7631=CARTESIAN_POINT('Origin',(-149.,49.,19.));
#7632=CARTESIAN_POINT('Origin',(-149.,49.,0.));
#7633=CARTESIAN_POINT('',(-149.,50.,-20.));
#7634=CARTESIAN_POINT('',(-149.,50.,0.));
#7635=CARTESIAN_POINT('Origin',(-149.,49.,-19.));
#7636=CARTESIAN_POINT('Origin',(-149.,25.,19.));
#7637=CARTESIAN_POINT('',(-149.,25.,20.));
#7638=CARTESIAN_POINT('Origin',(-135.,49.,19.));
#7639=CARTESIAN_POINT('',(-135.,50.,19.));
#7640=CARTESIAN_POINT('Origin',(-149.,25.,-19.));
#7641=CARTESIAN_POINT('',(-149.,25.,-20.));
#7642=CARTESIAN_POINT('Origin',(-145.,-49.,-19.));
#7643=CARTESIAN_POINT('',(-145.,-49.,-20.));
#7644=CARTESIAN_POINT('',(-145.,-50.,-19.));
#7645=CARTESIAN_POINT('Origin',(-131.,-25.,-19.));
#7646=CARTESIAN_POINT('',(-130.,-25.,-19.));
#7647=CARTESIAN_POINT('',(-131.,-25.,-20.));
#7648=CARTESIAN_POINT('Origin',(-140.,8.88178419700125E-15,-20.));
#7649=CARTESIAN_POINT('',(-150.,50.,-20.));
#7650=CARTESIAN_POINT('Origin',(-130.,-50.,0.));
#7651=CARTESIAN_POINT('Origin',(-130.,-37.8343839603864,-7.99999999999999));
#7652=CARTESIAN_POINT('',(-130.,-7.50000000000001,1.14489504879301E-14));
#7653=CARTESIAN_POINT('Origin',(-130.,1.91963385766348E-15,1.05304653885696E-14));
#7654=CARTESIAN_POINT('Origin',(-150.,-50.,0.));
#7655=CARTESIAN_POINT('Origin',(-140.,8.88178419700125E-15,20.));
#7656=CARTESIAN_POINT('Origin',(0.,-37.8343839603864,-7.99999999999999));
#7657=CARTESIAN_POINT('Origin',(-140.,2.22044604925031E-15,9.99200722162641E-15));
#7658=CARTESIAN_POINT('',(-140.,-7.50000000000001,9.6119802892091E-15));
#7659=CARTESIAN_POINT('Origin',(-140.,1.91963385766348E-15,1.05304653885696E-14));
#7660=CARTESIAN_POINT('Origin',(0.,1.91963385766348E-15,1.05304653885696E-14));
#7661=CARTESIAN_POINT('',(0.,-7.50000000000001,9.61198028920908E-15));
#7662=CARTESIAN_POINT('Origin',(-130.,50.,0.));
#7663=CARTESIAN_POINT('',(0.,0.,0.));
#7664=CARTESIAN_POINT('Origin',(140.,37.8343839603864,-8.00000000000001));
#7665=CARTESIAN_POINT('',(140.,31.8343839603864,-8.00000000000001));
#7666=CARTESIAN_POINT('Origin',(140.,37.8343839603864,-8.00000000000001));
#7667=CARTESIAN_POINT('',(120.,31.8343839603864,-8.00000000000001));
#7668=CARTESIAN_POINT('',(140.,31.8343839603864,-8.00000000000001));
#7669=CARTESIAN_POINT('Origin',(120.,37.8343839603864,-8.00000000000001));
#7670=CARTESIAN_POINT('Origin',(140.,37.8343839603864,-8.00000000000001));
#7671=CARTESIAN_POINT('',(140.,34.8343839603864,-8.00000000000001));
#7672=CARTESIAN_POINT('Origin',(140.,37.8343839603864,-8.00000000000001));
#7673=CARTESIAN_POINT('Origin',(130.,23.6740181268338,20.));
#7674=CARTESIAN_POINT('',(126.,23.6740181268338,20.));
#7675=CARTESIAN_POINT('Origin',(130.,23.6740181268338,20.));
#7676=CARTESIAN_POINT('',(126.,23.6740181268338,-3.));
#7677=CARTESIAN_POINT('',(126.,23.6740181268338,20.));
#7678=CARTESIAN_POINT('Origin',(130.,23.6740181268338,-3.));
#7679=CARTESIAN_POINT('Origin',(130.,23.6740181268338,-3.));
#7680=CARTESIAN_POINT('Origin',(130.,-23.6740181268338,20.));
#7681=CARTESIAN_POINT('',(126.,-23.6740181268338,20.));
#7682=CARTESIAN_POINT('Origin',(130.,-23.6740181268338,20.));
#7683=CARTESIAN_POINT('',(126.,-23.6740181268338,-3.));
#7684=CARTESIAN_POINT('',(126.,-23.6740181268338,20.));
#7685=CARTESIAN_POINT('Origin',(130.,-23.6740181268338,-3.));
#7686=CARTESIAN_POINT('Origin',(130.,-23.6740181268338,-3.));
#7687=CARTESIAN_POINT('Origin',(150.,-37.8343839603864,-8.00000000000001));
#7688=CARTESIAN_POINT('',(150.,-42.8343839603862,-8.00000000000001));
#7689=CARTESIAN_POINT('Origin',(150.,-37.8343839603864,-8.00000000000001));
#7690=CARTESIAN_POINT('',(142.,-42.8343839603862,-8.00000000000001));
#7691=CARTESIAN_POINT('',(150.,-42.8343839603862,-8.00000000000001));
#7692=CARTESIAN_POINT('Origin',(142.,-37.8343839603864,-8.00000000000001));
#7693=CARTESIAN_POINT('Origin',(142.,-37.8343839603864,-8.00000000000001));
#7694=CARTESIAN_POINT('',(142.,-40.8343839603864,-8.00000000000001));
#7695=CARTESIAN_POINT('Origin',(142.,-37.8343839603864,-8.00000000000001));
#7696=CARTESIAN_POINT('Origin',(150.,37.8343839603864,-8.00000000000001));
#7697=CARTESIAN_POINT('',(150.,32.8343839603866,-8.00000000000001));
#7698=CARTESIAN_POINT('Origin',(150.,37.8343839603864,-8.00000000000001));
#7699=CARTESIAN_POINT('',(142.,32.8343839603866,-8.00000000000001));
#7700=CARTESIAN_POINT('',(150.,32.8343839603866,-8.00000000000001));
#7701=CARTESIAN_POINT('Origin',(142.,37.8343839603864,-8.00000000000001));
#7702=CARTESIAN_POINT('Origin',(142.,37.8343839603864,-8.00000000000001));
#7703=CARTESIAN_POINT('',(142.,34.8343839603864,-8.00000000000001));
#7704=CARTESIAN_POINT('Origin',(142.,37.8343839603864,-8.00000000000001));
#7705=CARTESIAN_POINT('Origin',(150.,37.8343839603864,-8.00000000000001));
#7706=CARTESIAN_POINT('',(150.,34.8343839603864,-8.00000000000001));
#7707=CARTESIAN_POINT('Origin',(150.,-37.8343839603864,-8.00000000000001));
#7708=CARTESIAN_POINT('',(140.,-40.8343839603864,-8.00000000000001));
#7709=CARTESIAN_POINT('',(150.,-40.8343839603864,-8.00000000000001));
#7710=CARTESIAN_POINT('Origin',(140.,-37.8343839603864,-8.00000000000001));
#7711=CARTESIAN_POINT('Origin',(121.,49.,-19.));
#7712=CARTESIAN_POINT('',(120.,49.,-19.));
#7713=CARTESIAN_POINT('',(121.,49.,-20.));
#7714=CARTESIAN_POINT('Origin',(121.,49.,-19.));
#7715=CARTESIAN_POINT('',(121.,50.,-19.));
#7716=CARTESIAN_POINT('Origin',(121.,49.,-19.));
#7717=CARTESIAN_POINT('Origin',(121.,49.,-19.));
#7718=CARTESIAN_POINT('Origin',(121.,-49.,-19.));
#7719=CARTESIAN_POINT('',(121.,-50.,-19.));
#7720=CARTESIAN_POINT('',(121.,-49.,-20.));
#7721=CARTESIAN_POINT('Origin',(121.,-49.,-19.));
#7722=CARTESIAN_POINT('',(120.,-49.,-19.));
#7723=CARTESIAN_POINT('Origin',(121.,-49.,-19.));
#7724=CARTESIAN_POINT('Origin',(121.,-49.,-19.));
#7725=CARTESIAN_POINT('Origin',(149.,49.,-19.));
#7726=CARTESIAN_POINT('',(149.,50.,-19.));
#7727=CARTESIAN_POINT('',(149.,49.,-20.));
#7728=CARTESIAN_POINT('Origin',(149.,49.,-19.));
#7729=CARTESIAN_POINT('',(150.,49.,-19.));
#7730=CARTESIAN_POINT('Origin',(149.,49.,-19.));
#7731=CARTESIAN_POINT('Origin',(149.,49.,-19.));
#7732=CARTESIAN_POINT('Origin',(121.,49.,19.));
#7733=CARTESIAN_POINT('',(121.,50.,19.));
#7734=CARTESIAN_POINT('',(121.,49.,20.));
#7735=CARTESIAN_POINT('Origin',(121.,49.,19.));
#7736=CARTESIAN_POINT('',(120.,49.,19.));
#7737=CARTESIAN_POINT('Origin',(121.,49.,19.));
#7738=CARTESIAN_POINT('Origin',(121.,49.,19.));
#7739=CARTESIAN_POINT('Origin',(121.,49.,0.));
#7740=CARTESIAN_POINT('',(121.,50.,0.));
#7741=CARTESIAN_POINT('',(120.,49.,0.));
#7742=CARTESIAN_POINT('Origin',(149.,-49.,-19.));
#7743=CARTESIAN_POINT('',(150.,-49.,-19.));
#7744=CARTESIAN_POINT('',(149.,-49.,-20.));
#7745=CARTESIAN_POINT('Origin',(149.,-49.,-19.));
#7746=CARTESIAN_POINT('',(149.,-50.,-19.));
#7747=CARTESIAN_POINT('Origin',(149.,-49.,-19.));
#7748=CARTESIAN_POINT('Origin',(149.,-49.,-19.));
#7749=CARTESIAN_POINT('Origin',(121.,-49.,19.));
#7750=CARTESIAN_POINT('',(120.,-49.,19.));
#7751=CARTESIAN_POINT('',(121.,-49.,20.));
#7752=CARTESIAN_POINT('Origin',(121.,-49.,19.));
#7753=CARTESIAN_POINT('',(121.,-50.,19.));
#7754=CARTESIAN_POINT('Origin',(121.,-49.,19.));
#7755=CARTESIAN_POINT('Origin',(121.,-49.,19.));
#7756=CARTESIAN_POINT('Origin',(121.,-49.,0.));
#7757=CARTESIAN_POINT('',(120.,-49.,0.));
#7758=CARTESIAN_POINT('',(121.,-50.,0.));
#7759=CARTESIAN_POINT('Origin',(149.,49.,19.));
#7760=CARTESIAN_POINT('',(150.,49.,19.));
#7761=CARTESIAN_POINT('',(149.,49.,20.));
#7762=CARTESIAN_POINT('Origin',(149.,49.,19.));
#7763=CARTESIAN_POINT('',(149.,50.,19.));
#7764=CARTESIAN_POINT('Origin',(149.,49.,19.));
#7765=CARTESIAN_POINT('Origin',(149.,49.,19.));
#7766=CARTESIAN_POINT('Origin',(149.,49.,0.));
#7767=CARTESIAN_POINT('',(150.,49.,0.));
#7768=CARTESIAN_POINT('',(149.,50.,0.));
#7769=CARTESIAN_POINT('Origin',(142.5,49.,19.));
#7770=CARTESIAN_POINT('',(142.5,49.,20.));
#7771=CARTESIAN_POINT('',(142.5,50.,19.));
#7772=CARTESIAN_POINT('Origin',(149.,-49.,19.));
#7773=CARTESIAN_POINT('',(149.,-50.,19.));
#7774=CARTESIAN_POINT('',(149.,-49.,20.));
#7775=CARTESIAN_POINT('Origin',(149.,-49.,19.));
#7776=CARTESIAN_POINT('',(150.,-49.,19.));
#7777=CARTESIAN_POINT('Origin',(149.,-49.,19.));
#7778=CARTESIAN_POINT('Origin',(149.,-49.,19.));
#7779=CARTESIAN_POINT('Origin',(149.,-49.,0.));
#7780=CARTESIAN_POINT('',(150.,-49.,0.));
#7781=CARTESIAN_POINT('',(149.,-50.,0.));
#7782=CARTESIAN_POINT('Origin',(149.,-25.,19.));
#7783=CARTESIAN_POINT('',(149.,-25.,20.));
#7784=CARTESIAN_POINT('',(150.,-25.,19.));
#7785=CARTESIAN_POINT('Origin',(127.5,-49.,19.));
#7786=CARTESIAN_POINT('',(127.5,-49.,20.));
#7787=CARTESIAN_POINT('',(127.5,-50.,19.));
#7788=CARTESIAN_POINT('Origin',(121.,25.,19.));
#7789=CARTESIAN_POINT('',(121.,25.,20.));
#7790=CARTESIAN_POINT('',(120.,25.,19.));
#7791=CARTESIAN_POINT('Origin',(127.5,-49.,-19.));
#7792=CARTESIAN_POINT('',(127.5,-49.,-20.));
#7793=CARTESIAN_POINT('',(127.5,-50.,-19.));
#7794=CARTESIAN_POINT('Origin',(149.,-25.,-19.));
#7795=CARTESIAN_POINT('',(149.,-25.,-20.));
#7796=CARTESIAN_POINT('',(150.,-25.,-19.));
#7797=CARTESIAN_POINT('Origin',(142.5,49.,-19.));
#7798=CARTESIAN_POINT('',(142.5,49.,-20.));
#7799=CARTESIAN_POINT('',(142.5,50.,-19.));
#7800=CARTESIAN_POINT('Origin',(121.,25.,-19.));
#7801=CARTESIAN_POINT('',(121.,25.,-20.));
#7802=CARTESIAN_POINT('',(120.,25.,-19.));
#7803=CARTESIAN_POINT('Origin',(120.,50.,0.));
#7804=CARTESIAN_POINT('',(120.,-7.50000000000001,9.6119802892091E-15));
#7805=CARTESIAN_POINT('Origin',(120.,1.91963385766348E-15,1.05304653885696E-14));
#7806=CARTESIAN_POINT('',(120.,-43.8343839603864,-7.99999999999999));
#7807=CARTESIAN_POINT('Origin',(120.,-37.8343839603864,-7.99999999999999));
#7808=CARTESIAN_POINT('Origin',(150.,50.,0.));
#7809=CARTESIAN_POINT('Origin',(135.,8.88178419700125E-15,20.));
#7810=CARTESIAN_POINT('Origin',(120.,-50.,0.));
#7811=CARTESIAN_POINT('Origin',(150.,-50.,0.));
#7812=CARTESIAN_POINT('Origin',(135.,8.88178419700125E-15,-20.));
#7813=CARTESIAN_POINT('Origin',(0.,-37.8343839603864,-7.99999999999999));
#7814=CARTESIAN_POINT('',(140.,-43.8343839603864,-7.99999999999999));
#7815=CARTESIAN_POINT('',(0.,-43.8343839603864,-7.99999999999999));
#7816=CARTESIAN_POINT('Origin',(140.,-37.8343839603864,-7.99999999999999));
#7817=CARTESIAN_POINT('Origin',(140.,-37.8343839603864,-7.99999999999999));
#7818=CARTESIAN_POINT('Origin',(0.,1.91963385766348E-15,1.05304653885696E-14));
#7819=CARTESIAN_POINT('',(140.,-7.50000000000001,9.6119802892091E-15));
#7820=CARTESIAN_POINT('',(0.,-7.50000000000001,9.61198028920908E-15));
#7821=CARTESIAN_POINT('Origin',(140.,1.91963385766348E-15,1.05304653885696E-14));
#7822=CARTESIAN_POINT('Origin',(140.,2.22044604925031E-15,9.99200722162641E-15));
#7823=CARTESIAN_POINT('',(0.,0.,0.));
#7824=CARTESIAN_POINT('Origin',(0.,0.,1.30104260698261E-15));
#7825=CARTESIAN_POINT('',(8.8786892938183E-16,7.24999999999999,-1.11111111111111));
#7826=CARTESIAN_POINT('Origin',(0.,2.55134749822366E-16,-1.11111111111111));
#7827=CARTESIAN_POINT('',(-8.8786892938183E-16,7.24999999999999,1.11111111111111));
#7828=CARTESIAN_POINT('Origin',(1.01033360929657E-15,8.25,-2.1445780696224E-16));
#7829=CARTESIAN_POINT('Origin',(0.,6.6335034953815E-16,1.11111111111111));
#7830=CARTESIAN_POINT('Origin',(0.,-4.26423346241407E-31,-2.5));
#7831=CARTESIAN_POINT('',(-7.34788079488412E-16,6.,-2.25000000000001));
#7832=CARTESIAN_POINT('Origin',(0.,4.5924254968025E-17,-2.25));
#7833=CARTESIAN_POINT('',(-7.65404249467094E-16,6.24999999999999,-2.5));
#7834=CARTESIAN_POINT('',(7.65404249467095E-16,6.24999999999999,-2.5));
#7835=CARTESIAN_POINT('Origin',(0.,-4.26423346241407E-31,-2.5));
#7836=CARTESIAN_POINT('Origin',(0.,0.,-2.5));
#7837=CARTESIAN_POINT('',(-7.34788079488412E-16,6.,2.25000000000001));
#7838=CARTESIAN_POINT('',(-7.34788079488412E-16,6.,-2.5));
#7839=CARTESIAN_POINT('',(7.50096164477753E-16,-6.,2.25000000000001));
#7840=CARTESIAN_POINT('Origin',(0.,8.7256084439249E-16,2.25000000000001));
#7841=CARTESIAN_POINT('Origin',(0.,8.7256084439249E-16,2.25000000000001));
#7842=CARTESIAN_POINT('Origin',(0.,8.7256084439249E-16,2.25000000000001));
#7843=CARTESIAN_POINT('',(-7.65404249467094E-16,-6.24999999999999,2.50000000000001));
#7844=CARTESIAN_POINT('',(7.34788079488412E-16,-6.,2.25000000000001));
#7845=CARTESIAN_POINT('Origin',(0.,9.18485099360516E-16,2.5));
#7846=CARTESIAN_POINT('Origin',(0.,0.,-2.5));
#7847=CARTESIAN_POINT('',(-8.8786892938183E-16,7.24999999999999,2.5));
#7848=CARTESIAN_POINT('Origin',(0.,9.18485099360516E-16,2.50000000000001));
#7849=CARTESIAN_POINT('',(-8.8786892938183E-16,7.24999999999999,-2.5));
#7850=CARTESIAN_POINT('Origin',(0.,0.,-2.5));
#7851=CARTESIAN_POINT('',(-8.8786892938183E-16,7.24999999999999,-2.5));
#7852=CARTESIAN_POINT('',(-8.8786892938183E-16,7.24999999999999,-2.5));
#7853=CARTESIAN_POINT('Origin',(0.,-3.92678751131515E-31,-2.5));
#7854=CARTESIAN_POINT('Origin',(0.,6.24999999999999,-2.5));
#7855=CARTESIAN_POINT('Origin',(0.,6.24999999999999,2.5));
#7856=CARTESIAN_POINT('Origin',(0.,8.25,0.));
#7857=CARTESIAN_POINT('',(-1.49484711634153,8.25,1.12095579315854E-32));
#7858=CARTESIAN_POINT('',(1.49484711634153,8.25,1.12095579315854E-32));
#7859=CARTESIAN_POINT('Origin',(0.,8.25,0.));
#7860=CARTESIAN_POINT('Origin',(0.,9.18485099360516E-16,2.5));
#7861=CARTESIAN_POINT('',(-1.28587913910472E-15,10.5,2.25000000000001));
#7862=CARTESIAN_POINT('Origin',(0.,8.72560844392491E-16,2.25000000000001));
#7863=CARTESIAN_POINT('',(-1.25526296912604E-15,10.25,2.5));
#7864=CARTESIAN_POINT('',(1.25526296912604E-15,10.25,2.5));
#7865=CARTESIAN_POINT('Origin',(0.,9.18485099360516E-16,2.5));
#7866=CARTESIAN_POINT('Origin',(0.,0.,-2.5));
#7867=CARTESIAN_POINT('',(-1.1327982892113E-15,9.25000000000001,1.11111111111111));
#7868=CARTESIAN_POINT('Origin',(0.,6.6335034953815E-16,1.11111111111111));
#7869=CARTESIAN_POINT('',(-1.1327982892113E-15,9.25000000000001,2.50000000000001));
#7870=CARTESIAN_POINT('',(-1.1327982892113E-15,9.25000000000001,-2.5));
#7871=CARTESIAN_POINT('Origin',(0.,9.18485099360517E-16,2.50000000000001));
#7872=CARTESIAN_POINT('Origin',(0.,0.,1.30104260698261E-15));
#7873=CARTESIAN_POINT('',(-1.1327982892113E-15,9.25,-1.11111111111111));
#7874=CARTESIAN_POINT('Origin',(1.01033360929657E-15,8.25,-2.1445780696224E-16));
#7875=CARTESIAN_POINT('Origin',(0.,2.55134749822365E-16,-1.11111111111111));
#7876=CARTESIAN_POINT('Origin',(0.,0.,-2.5));
#7877=CARTESIAN_POINT('',(-1.1327982892113E-15,9.25,-2.5));
#7878=CARTESIAN_POINT('Origin',(0.,6.30801037605615E-31,-2.5));
#7879=CARTESIAN_POINT('',(-1.1327982892113E-15,9.25,-2.5));
#7880=CARTESIAN_POINT('Origin',(0.,4.59242549680263E-17,-2.25));
#7881=CARTESIAN_POINT('',(1.28587913910472E-15,10.5,-2.25));
#7882=CARTESIAN_POINT('',(1.28587913910472E-15,-10.5,-2.25));
#7883=CARTESIAN_POINT('Origin',(0.,4.59242549680263E-17,-2.25));
#7884=CARTESIAN_POINT('Origin',(0.,4.59242549680263E-17,-2.25));
#7885=CARTESIAN_POINT('',(-1.25526296912604E-15,-10.25,-2.49999999999999));
#7886=CARTESIAN_POINT('',(1.28587913910472E-15,-10.5,-2.25));
#7887=CARTESIAN_POINT('Origin',(0.,9.83209165554622E-31,-2.5));
#7888=CARTESIAN_POINT('Origin',(0.,0.,-2.5));
#7889=CARTESIAN_POINT('',(-1.28587913910472E-15,10.5,-2.5));
#7890=CARTESIAN_POINT('Origin',(0.,10.25,-2.5));
#7891=CARTESIAN_POINT('Origin',(0.,10.25,2.5));
#7892=CARTESIAN_POINT('Origin',(4.12500000000001,7.14470958122162,2.03038556022778E-16));
#7893=CARTESIAN_POINT('',(2.83042442247433,7.89213313939239,6.57390758046047E-17));
#7894=CARTESIAN_POINT('',(5.41957557752569,6.39728602305085,3.40338036240951E-16));
#7895=CARTESIAN_POINT('Origin',(4.12500000000001,7.14470958122162,2.03038556022778E-16));
#7896=CARTESIAN_POINT('Origin',(7.14470958122163,4.12499999999998,7.57750206972428E-16));
#7897=CARTESIAN_POINT('',(6.39728602305087,5.41957557752566,5.19940531381754E-16));
#7898=CARTESIAN_POINT('',(7.89213313939239,2.8304244224743,9.95559882563102E-16));
#7899=CARTESIAN_POINT('Origin',(7.14470958122163,4.12499999999998,7.57750206972428E-16));
#7900=CARTESIAN_POINT('Origin',(8.25,-2.88047210454559E-14,1.51550041394486E-15));
#7901=CARTESIAN_POINT('',(8.25000000000001,1.4948471163415,1.24090145350851E-15));
#7902=CARTESIAN_POINT('',(8.24999999999999,-1.49484711634156,1.79009937438121E-15));
#7903=CARTESIAN_POINT('Origin',(8.25,-2.88047210454559E-14,1.51550041394486E-15));
#7904=CARTESIAN_POINT('Origin',(7.1447095812216,-4.12500000000003,2.27325062091728E-15));
#7905=CARTESIAN_POINT('',(7.89213313939237,-2.83042442247436,2.03544094532661E-15));
#7906=CARTESIAN_POINT('',(6.39728602305083,-5.4195755775257,2.51106029650795E-15));
#7907=CARTESIAN_POINT('Origin',(7.1447095812216,-4.12500000000003,2.27325062091728E-15));
#7908=CARTESIAN_POINT('Origin',(4.12499999999996,-7.14470958122164,2.82796227186693E-15));
#7909=CARTESIAN_POINT('',(5.41957557752564,-6.39728602305088,2.69066279164876E-15));
#7910=CARTESIAN_POINT('',(2.83042442247428,-7.8921331393924,2.9652617520851E-15));
#7911=CARTESIAN_POINT('Origin',(4.12499999999996,-7.14470958122164,2.82796227186693E-15));
#7912=CARTESIAN_POINT('Origin',(0.,-8.25,3.0310008278897E-15));
#7913=CARTESIAN_POINT('',(1.49484711634153,-8.25,3.0310008278897E-15));
#7914=CARTESIAN_POINT('',(-1.49484711634153,-8.25,3.0310008278897E-15));
#7915=CARTESIAN_POINT('Origin',(0.,-8.25,3.0310008278897E-15));
#7916=CARTESIAN_POINT('Origin',(-4.12500000000006,-7.14470958122159,2.82796227186692E-15));
#7917=CARTESIAN_POINT('',(-2.83042442247439,-7.89213313939237,2.9652617520851E-15));
#7918=CARTESIAN_POINT('',(-5.41957557752573,-6.39728602305081,2.69066279164875E-15));
#7919=CARTESIAN_POINT('Origin',(-4.12500000000006,-7.14470958122159,2.82796227186692E-15));
#7920=CARTESIAN_POINT('Origin',(-7.14470958122166,-4.12499999999993,2.27325062091726E-15));
#7921=CARTESIAN_POINT('',(-6.39728602305091,-5.41957557752561,2.51106029650794E-15));
#7922=CARTESIAN_POINT('',(-7.89213313939241,-2.83042442247425,2.03544094532659E-15));
#7923=CARTESIAN_POINT('Origin',(-7.14470958122166,-4.12499999999993,2.27325062091726E-15));
#7924=CARTESIAN_POINT('Origin',(-8.25,8.64141631363676E-14,1.51550041394483E-15));
#7925=CARTESIAN_POINT('',(-8.25000000000002,-1.49484711634144,1.79009937438118E-15));
#7926=CARTESIAN_POINT('',(-8.24999999999999,1.49484711634162,1.24090145350848E-15));
#7927=CARTESIAN_POINT('Origin',(-8.25,8.64141631363676E-14,1.51550041394483E-15));
#7928=CARTESIAN_POINT('Ctrl Pts',(1.43761115075249E-15,8.75,1.59062243825056));
#7929=CARTESIAN_POINT('Ctrl Pts',(-1.59062243825055,8.75000000000001,1.59062243825056));
#7930=CARTESIAN_POINT('Ctrl Pts',(-1.59062243825055,8.75000000000003,6.65240462528331E-15));
#7931=CARTESIAN_POINT('Ctrl Pts',(-1.59062243825055,8.75000000000005,-1.59062243825054));
#7932=CARTESIAN_POINT('Ctrl Pts',(1.43761115075249E-15,8.75000000000005,
-1.59062243825054));
#7933=CARTESIAN_POINT('Ctrl Pts',(1.59062243825055,8.75000000000004,-1.59062243825054));
#7934=CARTESIAN_POINT('Ctrl Pts',(1.59062243825055,8.75000000000002,6.65240462528319E-15));
#7935=CARTESIAN_POINT('Ctrl Pts',(1.59062243825055,8.75,1.59062243825056));
#7936=CARTESIAN_POINT('Ctrl Pts',(1.43761115075249E-15,8.75,1.59062243825056));
#7937=CARTESIAN_POINT('Ctrl Pts',(1.46367293285559E-17,8.24999999999998,
1.77871997289447));
#7938=CARTESIAN_POINT('Ctrl Pts',(-1.77871997289447,8.24999999999998,1.77871997289447));
#7939=CARTESIAN_POINT('Ctrl Pts',(-1.77871997289447,8.25000000000001,-4.8572257327343E-16));
#7940=CARTESIAN_POINT('Ctrl Pts',(-1.77871997289447,8.25000000000003,-1.77871997289447));
#7941=CARTESIAN_POINT('Ctrl Pts',(1.46367293285536E-17,8.25000000000003,
-1.77871997289447));
#7942=CARTESIAN_POINT('Ctrl Pts',(1.77871997289447,8.25000000000002,-1.77871997289447));
#7943=CARTESIAN_POINT('Ctrl Pts',(1.77871997289447,8.24999999999999,-4.85722573273578E-16));
#7944=CARTESIAN_POINT('Ctrl Pts',(1.77871997289447,8.24999999999997,1.77871997289447));
#7945=CARTESIAN_POINT('Ctrl Pts',(1.46367293285559E-17,8.24999999999998,
1.77871997289447));
#7946=CARTESIAN_POINT('Ctrl Pts',(-1.40833769209538E-15,7.74999999999995,
1.59062243825054));
#7947=CARTESIAN_POINT('Ctrl Pts',(-1.59062243825055,7.74999999999996,1.59062243825054));
#7948=CARTESIAN_POINT('Ctrl Pts',(-1.59062243825055,7.74999999999998,-7.62384977183021E-15));
#7949=CARTESIAN_POINT('Ctrl Pts',(-1.59062243825055,7.75,-1.59062243825056));
#7950=CARTESIAN_POINT('Ctrl Pts',(-1.40833769209538E-15,7.75,-1.59062243825056));
#7951=CARTESIAN_POINT('Ctrl Pts',(1.59062243825055,7.74999999999999,-1.59062243825056));
#7952=CARTESIAN_POINT('Ctrl Pts',(1.59062243825055,7.74999999999997,-7.62384977183034E-15));
#7953=CARTESIAN_POINT('Ctrl Pts',(1.59062243825055,7.74999999999995,1.59062243825054));
#7954=CARTESIAN_POINT('Ctrl Pts',(-1.40833769209538E-15,7.74999999999995,
1.59062243825054));
#7955=CARTESIAN_POINT('',(-1.9479506776555E-16,7.75,1.59062243825056));
#7956=CARTESIAN_POINT('Origin',(0.,7.75,0.));
#7957=CARTESIAN_POINT('',(-1.9479506776555E-16,8.75,1.59062243825056));
#7958=CARTESIAN_POINT('Origin',(-1.7390814467874E-17,8.25,0.261524741817209));
#7959=CARTESIAN_POINT('Origin',(0.,8.75,0.));
#7960=CARTESIAN_POINT('Origin',(0.,8.25,-5.52943107967607E-15));
#7961=CARTESIAN_POINT('',(-1.49484711634152,8.25,-5.34636510605184E-15));
#7962=CARTESIAN_POINT('',(1.49484711634152,8.25,-5.52943107967607E-15));
#7963=CARTESIAN_POINT('Origin',(0.,8.25,-5.52943107967607E-15));
#7964=CARTESIAN_POINT('',(0.,7.75,-1.40874692590067));
#7965=CARTESIAN_POINT('Origin',(0.,7.75,0.));
#7966=CARTESIAN_POINT('',(0.,8.75,-1.40874692590067));
#7967=CARTESIAN_POINT('Origin',(0.,8.75,0.));
#7968=CARTESIAN_POINT('Origin',(0.,8.75,-1.40874692590067));
#7969=CARTESIAN_POINT('Origin',(0.,7.75,-1.59062243825056));
#7970=CARTESIAN_POINT('Ctrl Pts',(4.37500000000006,7.57772228311413,1.59062243825047));
#7971=CARTESIAN_POINT('Ctrl Pts',(2.99748056064553,8.37303350223928,1.5906224382504));
#7972=CARTESIAN_POINT('Ctrl Pts',(2.99748056064553,8.37303350223915,-9.98890215194051E-14));
#7973=CARTESIAN_POINT('Ctrl Pts',(2.99748056064553,8.37303350223902,-1.5906224382506));
#7974=CARTESIAN_POINT('Ctrl Pts',(4.37500000000006,7.57772228311387,-1.59062243825054));
#7975=CARTESIAN_POINT('Ctrl Pts',(5.7525194393546,6.78241106398871,-1.59062243825047));
#7976=CARTESIAN_POINT('Ctrl Pts',(5.7525194393546,6.78241106398884,2.79353679939059E-14));
#7977=CARTESIAN_POINT('Ctrl Pts',(5.7525194393546,6.78241106398897,1.59062243825053));
#7978=CARTESIAN_POINT('Ctrl Pts',(4.37500000000006,7.57772228311413,1.59062243825047));
#7979=CARTESIAN_POINT('Ctrl Pts',(4.12500000000001,7.14470958122175,1.77871997289453));
#7980=CARTESIAN_POINT('Ctrl Pts',(2.58458331725451,8.03406956766891,1.77871997289446));
#7981=CARTESIAN_POINT('Ctrl Pts',(2.58458331725451,8.03406956766877,-7.20914159458848E-14));
#7982=CARTESIAN_POINT('Ctrl Pts',(2.58458331725451,8.03406956766863,-1.7787199728946));
#7983=CARTESIAN_POINT('Ctrl Pts',(4.12500000000001,7.14470958122147,-1.77871997289453));
#7984=CARTESIAN_POINT('Ctrl Pts',(5.6654166827455,6.25534959477431,-1.77871997289446));
#7985=CARTESIAN_POINT('Ctrl Pts',(5.6654166827455,6.25534959477445,7.01658728875515E-14));
#7986=CARTESIAN_POINT('Ctrl Pts',(5.6654166827455,6.25534959477459,1.7787199728946));
#7987=CARTESIAN_POINT('Ctrl Pts',(4.12500000000001,7.14470958122175,1.77871997289453));
#7988=CARTESIAN_POINT('Ctrl Pts',(3.87499999999995,6.71169687932936,1.59062243825053));
#7989=CARTESIAN_POINT('Ctrl Pts',(2.49748056064542,7.50700809845451,1.59062243825047));
#7990=CARTESIAN_POINT('Ctrl Pts',(2.49748056064542,7.50700809845438,-2.98609110522392E-14));
#7991=CARTESIAN_POINT('Ctrl Pts',(2.49748056064542,7.50700809845425,-1.59062243825053));
#7992=CARTESIAN_POINT('Ctrl Pts',(3.87499999999995,6.7116968793291,-1.59062243825046));
#7993=CARTESIAN_POINT('Ctrl Pts',(5.25251943935448,5.91638566020395,-1.5906224382504));
#7994=CARTESIAN_POINT('Ctrl Pts',(5.25251943935448,5.91638566020407,9.79634784610718E-14));
#7995=CARTESIAN_POINT('Ctrl Pts',(5.25251943935448,5.9163856602042,1.59062243825059));
#7996=CARTESIAN_POINT('Ctrl Pts',(3.87499999999995,6.71169687932936,1.59062243825053));
#7997=CARTESIAN_POINT('',(3.87500000000001,6.71169687932939,1.59062243825056));
#7998=CARTESIAN_POINT('Origin',(3.87500000000001,6.71169687932939,1.90733188991095E-16));
#7999=CARTESIAN_POINT('',(4.37500000000001,7.57772228311383,1.59062243825056));
#8000=CARTESIAN_POINT('Origin',(4.12500000000001,7.14470958122164,0.261524741817169));
#8001=CARTESIAN_POINT('Origin',(4.37500000000001,7.57772228311383,2.15343923054462E-16));
#8002=CARTESIAN_POINT('Origin',(4.12500000000001,7.14470958122162,-5.32639252365329E-15));
#8003=CARTESIAN_POINT('',(2.83042442247434,7.89213313939238,-5.23485953684118E-15));
#8004=CARTESIAN_POINT('',(5.41957557752568,6.39728602305086,-5.23485953684118E-15));
#8005=CARTESIAN_POINT('Origin',(4.12500000000001,7.14470958122162,-5.32639252365329E-15));
#8006=CARTESIAN_POINT('',(3.87500000000001,6.71169687932939,-1.40874692590067));
#8007=CARTESIAN_POINT('Origin',(3.87500000000001,6.71169687932939,1.90733188991095E-16));
#8008=CARTESIAN_POINT('',(4.37500000000001,7.57772228311383,-1.40874692590067));
#8009=CARTESIAN_POINT('Origin',(4.37500000000001,7.57772228311383,2.15343923054462E-16));
#8010=CARTESIAN_POINT('Origin',(4.37500000000001,7.57772228311383,-1.40874692590067));
#8011=CARTESIAN_POINT('Origin',(3.87500000000001,6.71169687932939,-1.59062243825056));
#8012=CARTESIAN_POINT('Ctrl Pts',(7.57772228311385,4.37500000000001,-1.59062243825054));
#8013=CARTESIAN_POINT('Ctrl Pts',(8.37303350223914,2.99748056064552,-1.59062243825056));
#8014=CARTESIAN_POINT('Ctrl Pts',(8.37303350223917,2.99748056064552,-2.03075013256419E-14));
#8015=CARTESIAN_POINT('Ctrl Pts',(8.3730335022392,2.99748056064552,1.59062243825052));
#8016=CARTESIAN_POINT('Ctrl Pts',(7.57772228311391,4.37500000000001,1.59062243825053));
#8017=CARTESIAN_POINT('Ctrl Pts',(6.78241106398862,5.75251943935451,1.59062243825055));
#8018=CARTESIAN_POINT('Ctrl Pts',(6.78241106398859,5.75251943935451,1.063000168243E-14));
#8019=CARTESIAN_POINT('Ctrl Pts',(6.78241106398856,5.75251943935451,-1.59062243825053));
#8020=CARTESIAN_POINT('Ctrl Pts',(7.57772228311385,4.37500000000001,-1.59062243825054));
#8021=CARTESIAN_POINT('Ctrl Pts',(7.1447095812216,4.12499999999999,-1.77871997289447));
#8022=CARTESIAN_POINT('Ctrl Pts',(8.03406956766886,2.58458331725462,-1.77871997289449));
#8023=CARTESIAN_POINT('Ctrl Pts',(8.03406956766889,2.58458331725462,-1.42717923056121E-14));
#8024=CARTESIAN_POINT('Ctrl Pts',(8.03406956766893,2.58458331725462,1.77871997289446));
#8025=CARTESIAN_POINT('Ctrl Pts',(7.14470958122166,4.12499999999999,1.77871997289448));
#8026=CARTESIAN_POINT('Ctrl Pts',(6.2553495947744,5.66541668274535,1.7787199728945));
#8027=CARTESIAN_POINT('Ctrl Pts',(6.25534959477437,5.66541668274535,2.11066028009605E-14));
#8028=CARTESIAN_POINT('Ctrl Pts',(6.25534959477433,5.66541668274535,-1.77871997289445));
#8029=CARTESIAN_POINT('Ctrl Pts',(7.1447095812216,4.12499999999999,-1.77871997289447));
#8030=CARTESIAN_POINT('Ctrl Pts',(6.71169687932935,3.87499999999996,-1.59062243825053));
#8031=CARTESIAN_POINT('Ctrl Pts',(7.50700809845464,2.49748056064546,-1.59062243825054));
#8032=CARTESIAN_POINT('Ctrl Pts',(7.50700809845467,2.49748056064546,-4.35030269939418E-15));
#8033=CARTESIAN_POINT('Ctrl Pts',(7.5070080984547,2.49748056064546,1.59062243825054));
#8034=CARTESIAN_POINT('Ctrl Pts',(6.71169687932941,3.87499999999996,1.59062243825055));
#8035=CARTESIAN_POINT('Ctrl Pts',(5.91638566020411,5.25251943935446,1.59062243825057));
#8036=CARTESIAN_POINT('Ctrl Pts',(5.91638566020408,5.25251943935446,2.76974233333029E-14));
#8037=CARTESIAN_POINT('Ctrl Pts',(5.91638566020405,5.25251943935446,-1.59062243825051));
#8038=CARTESIAN_POINT('Ctrl Pts',(6.71169687932935,3.87499999999996,-1.59062243825053));
#8039=CARTESIAN_POINT('',(6.7116968793294,3.87499999999999,-1.59062243825056));
#8040=CARTESIAN_POINT('Origin',(6.71169687932941,3.87499999999998,7.11825952004402E-16));
#8041=CARTESIAN_POINT('',(7.57772228311384,4.37500000000001,-1.59062243825056));
#8042=CARTESIAN_POINT('Origin',(7.14470958122162,4.12499999999998,-0.261524741817215));
#8043=CARTESIAN_POINT('Origin',(7.57772228311385,4.37499999999998,8.03674461940454E-16));
#8044=CARTESIAN_POINT('Origin',(7.14470958122163,4.12499999999998,-4.77168087270365E-15));
#8045=CARTESIAN_POINT('',(6.39728602305087,5.41957557752565,-4.68014788589154E-15));
#8046=CARTESIAN_POINT('',(7.89213313939239,2.83042442247431,-4.68014788589154E-15));
#8047=CARTESIAN_POINT('Origin',(7.14470958122163,4.12499999999998,-4.77168087270365E-15));
#8048=CARTESIAN_POINT('',(6.71169687932941,3.87499999999998,-1.40874692590067));
#8049=CARTESIAN_POINT('Origin',(6.71169687932941,3.87499999999998,7.11825952004402E-16));
#8050=CARTESIAN_POINT('',(7.57772228311385,4.37499999999998,-1.40874692590067));
#8051=CARTESIAN_POINT('Origin',(7.57772228311385,4.37499999999998,8.03674461940454E-16));
#8052=CARTESIAN_POINT('Origin',(7.57772228311385,4.37499999999998,-1.40874692590067));
#8053=CARTESIAN_POINT('Origin',(6.71169687932941,3.87499999999998,-1.59062243825056));
#8054=CARTESIAN_POINT('Ctrl Pts',(8.7500000000001,-3.01501838019841E-14,
-1.59062243825053));
#8055=CARTESIAN_POINT('Ctrl Pts',(8.75000000000009,-1.59062243825058,-1.59062243825053));
#8056=CARTESIAN_POINT('Ctrl Pts',(8.75000000000004,-1.59062243825058,1.7123474122469E-14));
#8057=CARTESIAN_POINT('Ctrl Pts',(8.75,-1.59062243825058,1.59062243825056));
#8058=CARTESIAN_POINT('Ctrl Pts',(8.75,-3.01501838019841E-14,1.59062243825056));
#8059=CARTESIAN_POINT('Ctrl Pts',(8.75000000000001,1.59062243825052,1.59062243825056));
#8060=CARTESIAN_POINT('Ctrl Pts',(8.75000000000006,1.59062243825052,1.71234741224694E-14));
#8061=CARTESIAN_POINT('Ctrl Pts',(8.7500000000001,1.59062243825052,-1.59062243825053));
#8062=CARTESIAN_POINT('Ctrl Pts',(8.7500000000001,-3.01501838019841E-14,
-1.59062243825053));
#8063=CARTESIAN_POINT('Ctrl Pts',(8.25000000000005,-2.83665235398244E-14,
-1.77871997289448));
#8064=CARTESIAN_POINT('Ctrl Pts',(8.25000000000005,-1.77871997289451,-1.77871997289448));
#8065=CARTESIAN_POINT('Ctrl Pts',(8.24999999999999,-1.77871997289451,2.08166817117158E-15));
#8066=CARTESIAN_POINT('Ctrl Pts',(8.24999999999994,-1.77871997289451,1.77871997289448));
#8067=CARTESIAN_POINT('Ctrl Pts',(8.24999999999995,-2.83665235398245E-14,
1.77871997289448));
#8068=CARTESIAN_POINT('Ctrl Pts',(8.24999999999995,1.77871997289445,1.77871997289448));
#8069=CARTESIAN_POINT('Ctrl Pts',(8.25000000000001,1.77871997289445,2.08166817117197E-15));
#8070=CARTESIAN_POINT('Ctrl Pts',(8.25000000000006,1.77871997289445,-1.77871997289448));
#8071=CARTESIAN_POINT('Ctrl Pts',(8.25000000000005,-2.83665235398244E-14,
-1.77871997289448));
#8072=CARTESIAN_POINT('Ctrl Pts',(7.75,-2.65828632776648E-14,-1.59062243825055));
#8073=CARTESIAN_POINT('Ctrl Pts',(7.75,-1.59062243825056,-1.59062243825055));
#8074=CARTESIAN_POINT('Ctrl Pts',(7.74999999999995,-1.59062243825056,-1.29601377801257E-14));
#8075=CARTESIAN_POINT('Ctrl Pts',(7.7499999999999,-1.59062243825056,1.59062243825052));
#8076=CARTESIAN_POINT('Ctrl Pts',(7.74999999999991,-2.65828632776648E-14,
1.59062243825052));
#8077=CARTESIAN_POINT('Ctrl Pts',(7.74999999999991,1.59062243825051,1.59062243825052));
#8078=CARTESIAN_POINT('Ctrl Pts',(7.74999999999996,1.59062243825051,-1.29601377801253E-14));
#8079=CARTESIAN_POINT('Ctrl Pts',(7.75000000000001,1.59062243825051,-1.59062243825055));
#8080=CARTESIAN_POINT('Ctrl Pts',(7.75,-2.65828632776648E-14,-1.59062243825055));
#8081=CARTESIAN_POINT('',(7.75,-2.67776583454304E-14,-1.59062243825056));
#8082=CARTESIAN_POINT('Origin',(7.75,-2.70589803760343E-14,1.4236519040088E-15));
#8083=CARTESIAN_POINT('',(8.75,-3.03449788697493E-14,-1.59062243825056));
#8084=CARTESIAN_POINT('Origin',(8.25000000000002,-2.83985510836209E-14,
-0.261524741817196));
#8085=CARTESIAN_POINT('Origin',(8.75,-3.05504617148774E-14,1.60734892388091E-15));
#8086=CARTESIAN_POINT('Origin',(8.25,-2.88047210454559E-14,-4.01393066573122E-15));
#8087=CARTESIAN_POINT('',(8.25000000000001,1.49484711634149,-4.10546365254334E-15));
#8088=CARTESIAN_POINT('',(8.24999999999999,-1.49484711634155,-3.73933170529488E-15));
#8089=CARTESIAN_POINT('Origin',(8.25,-2.88047210454559E-14,-4.01393066573122E-15));
#8090=CARTESIAN_POINT('',(7.75,-2.73177629880762E-14,-1.40874692590067));
#8091=CARTESIAN_POINT('Origin',(7.75,-2.70589803760343E-14,1.4236519040088E-15));
#8092=CARTESIAN_POINT('',(8.75,-3.08092443269194E-14,-1.40874692590067));
#8093=CARTESIAN_POINT('Origin',(8.75,-3.05504617148774E-14,1.60734892388091E-15));
#8094=CARTESIAN_POINT('Origin',(8.75,-3.08092443269194E-14,-1.40874692590067));
#8095=CARTESIAN_POINT('Origin',(7.75,-2.73511729776826E-14,-1.59062243825056));
#8096=CARTESIAN_POINT('Ctrl Pts',(7.57772228311398,-4.37500000000007,-1.5906224382505));
#8097=CARTESIAN_POINT('Ctrl Pts',(6.78241106398874,-5.75251943935458,-1.59062243825054));
#8098=CARTESIAN_POINT('Ctrl Pts',(6.78241106398865,-5.75251943935458,-1.83119572337645E-14));
#8099=CARTESIAN_POINT('Ctrl Pts',(6.78241106398857,-5.75251943935458,1.59062243825051));
#8100=CARTESIAN_POINT('Ctrl Pts',(7.57772228311382,-4.37500000000007,1.59062243825055));
#8101=CARTESIAN_POINT('Ctrl Pts',(8.37303350223906,-2.99748056064556,1.59062243825059));
#8102=CARTESIAN_POINT('Ctrl Pts',(8.37303350223915,-2.99748056064556,6.49547696131205E-14));
#8103=CARTESIAN_POINT('Ctrl Pts',(8.37303350223923,-2.99748056064556,-1.59062243825046));
#8104=CARTESIAN_POINT('Ctrl Pts',(7.57772228311398,-4.37500000000007,-1.5906224382505));
#8105=CARTESIAN_POINT('Ctrl Pts',(7.1447095812217,-4.12500000000003,-1.7787199728945));
#8106=CARTESIAN_POINT('Ctrl Pts',(6.25534959477447,-5.66541668274545,-1.77871997289454));
#8107=CARTESIAN_POINT('Ctrl Pts',(6.25534959477437,-5.66541668274545,-4.55067786765486E-14));
#8108=CARTESIAN_POINT('Ctrl Pts',(6.25534959477428,-5.66541668274545,1.77871997289445));
#8109=CARTESIAN_POINT('Ctrl Pts',(7.14470958122151,-4.12500000000003,1.7787199728945));
#8110=CARTESIAN_POINT('Ctrl Pts',(8.03406956766874,-2.58458331725462,1.77871997289454));
#8111=CARTESIAN_POINT('Ctrl Pts',(8.03406956766883,-2.58458331725462,4.67904740487708E-14));
#8112=CARTESIAN_POINT('Ctrl Pts',(8.03406956766892,-2.58458331725462,-1.77871997289445));
#8113=CARTESIAN_POINT('Ctrl Pts',(7.1447095812217,-4.12500000000003,-1.7787199728945));
#8114=CARTESIAN_POINT('Ctrl Pts',(6.71169687932939,-3.875,-1.59062243825054));
#8115=CARTESIAN_POINT('Ctrl Pts',(5.91638566020415,-5.2525194393545,-1.59062243825058));
#8116=CARTESIAN_POINT('Ctrl Pts',(5.91638566020406,-5.2525194393545,-6.31903335693023E-14));
#8117=CARTESIAN_POINT('Ctrl Pts',(5.91638566020398,-5.2525194393545,1.59062243825046));
#8118=CARTESIAN_POINT('Ctrl Pts',(6.71169687932922,-3.875,1.5906224382505));
#8119=CARTESIAN_POINT('Ctrl Pts',(7.50700809845447,-2.49748056064549,1.59062243825054));
#8120=CARTESIAN_POINT('Ctrl Pts',(7.50700809845455,-2.49748056064549,1.91149119343909E-14));
#8121=CARTESIAN_POINT('Ctrl Pts',(7.50700809845463,-2.49748056064549,-1.5906224382505));
#8122=CARTESIAN_POINT('Ctrl Pts',(6.71169687932939,-3.875,-1.59062243825054));
#8123=CARTESIAN_POINT('',(6.7116968793294,-3.875,-1.59062243825056));
#8124=CARTESIAN_POINT('Origin',(6.71169687932938,-3.87500000000003,2.1354778560132E-15));
#8125=CARTESIAN_POINT('',(7.57772228311385,-4.37499999999999,-1.59062243825056));
#8126=CARTESIAN_POINT('Origin',(7.14470958122162,-4.12500000000004,-0.261524741817231));
#8127=CARTESIAN_POINT('Origin',(7.57772228311382,-4.37500000000004,2.41102338582136E-15));
#8128=CARTESIAN_POINT('Origin',(7.1447095812216,-4.12500000000003,-3.25618045875879E-15));
#8129=CARTESIAN_POINT('',(7.89213313939237,-2.83042442247437,-3.16464747194668E-15));
#8130=CARTESIAN_POINT('',(6.39728602305083,-5.41957557752569,-3.16464747194668E-15));
#8131=CARTESIAN_POINT('Origin',(7.1447095812216,-4.12500000000003,-3.25618045875879E-15));
#8132=CARTESIAN_POINT('',(6.71169687932938,-3.87500000000003,-1.40874692590067));
#8133=CARTESIAN_POINT('Origin',(6.71169687932938,-3.87500000000003,2.1354778560132E-15));
#8134=CARTESIAN_POINT('',(7.57772228311382,-4.37500000000004,-1.40874692590067));
#8135=CARTESIAN_POINT('Origin',(7.57772228311382,-4.37500000000004,2.41102338582136E-15));
#8136=CARTESIAN_POINT('Origin',(7.57772228311382,-4.37500000000004,-1.40874692590067));
#8137=CARTESIAN_POINT('Origin',(6.71169687932938,-3.87500000000003,-1.59062243825055));
#8138=CARTESIAN_POINT('Ctrl Pts',(4.37499999999984,-7.57772228311397,-1.59062243825053));
#8139=CARTESIAN_POINT('Ctrl Pts',(2.99748056064537,-8.37303350223927,-1.59062243825036));
#8140=CARTESIAN_POINT('Ctrl Pts',(2.99748056064557,-8.37303350223927,1.48340183158392E-13));
#8141=CARTESIAN_POINT('Ctrl Pts',(2.99748056064577,-8.37303350223927,1.59062243825066));
#8142=CARTESIAN_POINT('Ctrl Pts',(4.37500000000023,-7.57772228311397,1.59062243825049));
#8143=CARTESIAN_POINT('Ctrl Pts',(5.7525194393547,-6.78241106398868,1.59062243825031));
#8144=CARTESIAN_POINT('Ctrl Pts',(5.7525194393545,-6.78241106398868,-1.96831619047452E-13));
#8145=CARTESIAN_POINT('Ctrl Pts',(5.7525194393543,-6.78241106398868,-1.59062243825071));
#8146=CARTESIAN_POINT('Ctrl Pts',(4.37499999999984,-7.57772228311397,-1.59062243825053));
#8147=CARTESIAN_POINT('Ctrl Pts',(4.12499999999973,-7.14470958122165,-1.7787199728945));
#8148=CARTESIAN_POINT('Ctrl Pts',(2.58458331725435,-8.03406956766895,-1.77871997289431));
#8149=CARTESIAN_POINT('Ctrl Pts',(2.58458331725457,-8.03406956766895,1.99898049178834E-13));
#8150=CARTESIAN_POINT('Ctrl Pts',(2.58458331725479,-8.03406956766895,1.77871997289471));
#8151=CARTESIAN_POINT('Ctrl Pts',(4.12500000000018,-7.14470958122165,1.77871997289452));
#8152=CARTESIAN_POINT('Ctrl Pts',(5.66541668274557,-6.25534959477435,1.77871997289432));
#8153=CARTESIAN_POINT('Ctrl Pts',(5.66541668274534,-6.25534959477435,-1.85655969441064E-13));
#8154=CARTESIAN_POINT('Ctrl Pts',(5.66541668274512,-6.25534959477435,-1.7787199728947));
#8155=CARTESIAN_POINT('Ctrl Pts',(4.12499999999973,-7.14470958122165,-1.7787199728945));
#8156=CARTESIAN_POINT('Ctrl Pts',(3.87499999999968,-6.71169687932932,-1.59062243825047));
#8157=CARTESIAN_POINT('Ctrl Pts',(2.49748056064522,-7.50700809845462,-1.5906224382503));
#8158=CARTESIAN_POINT('Ctrl Pts',(2.49748056064542,-7.50700809845462,2.11073698785222E-13));
#8159=CARTESIAN_POINT('Ctrl Pts',(2.49748056064561,-7.50700809845462,1.59062243825072));
#8160=CARTESIAN_POINT('Ctrl Pts',(3.87500000000008,-6.71169687932932,1.59062243825055));
#8161=CARTESIAN_POINT('Ctrl Pts',(5.25251943935454,-5.91638566020402,1.59062243825038));
#8162=CARTESIAN_POINT('Ctrl Pts',(5.25251943935434,-5.91638566020402,-1.34098103420622E-13));
#8163=CARTESIAN_POINT('Ctrl Pts',(5.25251943935414,-5.91638566020402,-1.59062243825064));
#8164=CARTESIAN_POINT('Ctrl Pts',(3.87499999999968,-6.71169687932932,-1.59062243825047));
#8165=CARTESIAN_POINT('',(3.87499999999979,-6.71169687932952,-1.59062243825056));
#8166=CARTESIAN_POINT('Origin',(3.87499999999996,-6.71169687932942,2.65657061902651E-15));
#8167=CARTESIAN_POINT('',(4.37499999999982,-7.57772228311395,-1.59062243825056));
#8168=CARTESIAN_POINT('Origin',(4.12499999999992,-7.14470958122165,-0.261524741817159));
#8169=CARTESIAN_POINT('Origin',(4.37499999999996,-7.57772228311387,2.99935392470735E-15));
#8170=CARTESIAN_POINT('Origin',(4.12499999999996,-7.14470958122164,-2.70146880780915E-15));
#8171=CARTESIAN_POINT('',(5.41957557752563,-6.39728602305089,-3.16504733330961E-15));
#8172=CARTESIAN_POINT('',(2.83042442247429,-7.89213313939239,-2.05482430868446E-15));
#8173=CARTESIAN_POINT('Origin',(4.12499999999996,-7.14470958122164,-2.70146880780915E-15));
#8174=CARTESIAN_POINT('',(3.87499999999996,-6.71169687932942,-1.40874692590067));
#8175=CARTESIAN_POINT('Origin',(3.87499999999996,-6.71169687932942,2.65657061902651E-15));
#8176=CARTESIAN_POINT('',(4.37499999999996,-7.57772228311387,-1.40874692590067));
#8177=CARTESIAN_POINT('Origin',(4.37499999999996,-7.57772228311387,2.99935392470735E-15));
#8178=CARTESIAN_POINT('Origin',(4.37499999999996,-7.57772228311387,-1.40874692590067));
#8179=CARTESIAN_POINT('Origin',(3.87499999999996,-6.71169687932942,-1.59062243825055));
#8180=CARTESIAN_POINT('Ctrl Pts',(3.82926740629614E-15,-8.75000000000001,
-1.59062243825056));
#8181=CARTESIAN_POINT('Ctrl Pts',(-1.59062243825054,-8.75000000000002,-1.59062243825056));
#8182=CARTESIAN_POINT('Ctrl Pts',(-1.59062243825054,-8.75000000000005,-9.87978730961784E-15));
#8183=CARTESIAN_POINT('Ctrl Pts',(-1.59062243825054,-8.75000000000008,1.59062243825054));
#8184=CARTESIAN_POINT('Ctrl Pts',(3.82926740629613E-15,-8.75000000000007,
1.59062243825054));
#8185=CARTESIAN_POINT('Ctrl Pts',(1.59062243825055,-8.75000000000006,1.59062243825054));
#8186=CARTESIAN_POINT('Ctrl Pts',(1.59062243825055,-8.75000000000003,-9.87978730961739E-15));
#8187=CARTESIAN_POINT('Ctrl Pts',(1.59062243825055,-8.75,-1.59062243825056));
#8188=CARTESIAN_POINT('Ctrl Pts',(3.82926740629614E-15,-8.75000000000001,
-1.59062243825056));
#8189=CARTESIAN_POINT('Ctrl Pts',(1.01372903127415E-16,-8.24999999999997,
-1.77871997289448));
#8190=CARTESIAN_POINT('Ctrl Pts',(-1.77871997289448,-8.24999999999998,-1.77871997289448));
#8191=CARTESIAN_POINT('Ctrl Pts',(-1.77871997289448,-8.25000000000001,-3.20923843056017E-16));
#8192=CARTESIAN_POINT('Ctrl Pts',(-1.77871997289448,-8.25000000000005,1.77871997289448));
#8193=CARTESIAN_POINT('Ctrl Pts',(1.01372903127413E-16,-8.25000000000004,
1.77871997289448));
#8194=CARTESIAN_POINT('Ctrl Pts',(1.77871997289448,-8.25000000000002,1.77871997289448));
#8195=CARTESIAN_POINT('Ctrl Pts',(1.77871997289448,-8.24999999999999,-3.20923843055502E-16));
#8196=CARTESIAN_POINT('Ctrl Pts',(1.77871997289448,-8.24999999999995,-1.77871997289448));
#8197=CARTESIAN_POINT('Ctrl Pts',(1.01372903127415E-16,-8.24999999999997,
-1.77871997289448));
#8198=CARTESIAN_POINT('Ctrl Pts',(-3.6265216000413E-15,-7.74999999999993,
-1.59062243825054));
#8199=CARTESIAN_POINT('Ctrl Pts',(-1.59062243825055,-7.74999999999995,-1.59062243825054));
#8200=CARTESIAN_POINT('Ctrl Pts',(-1.59062243825055,-7.74999999999998,9.23793962350586E-15));
#8201=CARTESIAN_POINT('Ctrl Pts',(-1.59062243825055,-7.75000000000001,1.59062243825056));
#8202=CARTESIAN_POINT('Ctrl Pts',(-3.62652160004131E-15,-7.74999999999999,
1.59062243825056));
#8203=CARTESIAN_POINT('Ctrl Pts',(1.59062243825055,-7.74999999999998,1.59062243825056));
#8204=CARTESIAN_POINT('Ctrl Pts',(1.59062243825055,-7.74999999999995,9.23793962350631E-15));
#8205=CARTESIAN_POINT('Ctrl Pts',(1.59062243825055,-7.74999999999992,-1.59062243825054));
#8206=CARTESIAN_POINT('Ctrl Pts',(-3.6265216000413E-15,-7.74999999999993,
-1.59062243825054));
#8207=CARTESIAN_POINT('',(-3.82131666780635E-15,-7.75,-1.59062243825056));
#8208=CARTESIAN_POINT('Origin',(0.,-7.75,2.8473038080176E-15));
#8209=CARTESIAN_POINT('',(3.63447233853054E-15,-8.75,-1.59062243825056));
#8210=CARTESIAN_POINT('Origin',(6.9345359330968E-17,-8.24999999999999,-0.261524741817196));
#8211=CARTESIAN_POINT('Origin',(0.,-8.75,3.2146978477618E-15));
#8212=CARTESIAN_POINT('Origin',(0.,-8.25,-2.49843025178637E-15));
#8213=CARTESIAN_POINT('',(1.49484711634152,-8.25,-2.31536427816214E-15));
#8214=CARTESIAN_POINT('',(-1.49484711634152,-8.25,-2.49843025178637E-15));
#8215=CARTESIAN_POINT('Origin',(0.,-8.25,-2.49843025178637E-15));
#8216=CARTESIAN_POINT('',(0.,-7.75,-1.40874692590067));
#8217=CARTESIAN_POINT('Origin',(0.,-7.75,2.8473038080176E-15));
#8218=CARTESIAN_POINT('',(0.,-8.75,-1.40874692590067));
#8219=CARTESIAN_POINT('Origin',(0.,-8.75,3.2146978477618E-15));
#8220=CARTESIAN_POINT('Origin',(0.,-8.75,-1.40874692590067));
#8221=CARTESIAN_POINT('Origin',(0.,-7.75,-1.59062243825055));
#8222=CARTESIAN_POINT('Ctrl Pts',(-4.37500000000018,-7.57772228311385,1.59062243825053));
#8223=CARTESIAN_POINT('Ctrl Pts',(-2.9974805606457,-8.37303350223915,1.5906224382506));
#8224=CARTESIAN_POINT('Ctrl Pts',(-2.99748056064561,-8.37303350223915,6.28013398870636E-14));
#8225=CARTESIAN_POINT('Ctrl Pts',(-2.99748056064553,-8.37303350223915,-1.59062243825047));
#8226=CARTESIAN_POINT('Ctrl Pts',(-4.37500000000001,-7.57772228311385,-1.59062243825055));
#8227=CARTESIAN_POINT('Ctrl Pts',(-5.7525194393545,-6.78241106398854,-1.59062243825062));
#8228=CARTESIAN_POINT('Ctrl Pts',(-5.75251943935459,-6.78241106398854,-8.52667869644686E-14));
#8229=CARTESIAN_POINT('Ctrl Pts',(-5.75251943935467,-6.78241106398854,1.59062243825045));
#8230=CARTESIAN_POINT('Ctrl Pts',(-4.37500000000018,-7.57772228311385,1.59062243825053));
#8231=CARTESIAN_POINT('Ctrl Pts',(-4.12500000000016,-7.14470958122159,1.77871997289448));
#8232=CARTESIAN_POINT('Ctrl Pts',(-2.58458331725479,-8.03406956766887,1.77871997289457));
#8233=CARTESIAN_POINT('Ctrl Pts',(-2.58458331725469,-8.03406956766887,8.49165151811221E-14));
#8234=CARTESIAN_POINT('Ctrl Pts',(-2.5845833172546,-8.03406956766887,-1.7787199728944));
#8235=CARTESIAN_POINT('Ctrl Pts',(-4.12499999999996,-7.14470958122159,-1.77871997289448));
#8236=CARTESIAN_POINT('Ctrl Pts',(-5.66541668274533,-6.2553495947743,-1.77871997289456));
#8237=CARTESIAN_POINT('Ctrl Pts',(-5.66541668274543,-6.2553495947743,-8.04582758478618E-14));
#8238=CARTESIAN_POINT('Ctrl Pts',(-5.66541668274552,-6.2553495947743,1.7787199728944));
#8239=CARTESIAN_POINT('Ctrl Pts',(-4.12500000000016,-7.14470958122159,1.77871997289448));
#8240=CARTESIAN_POINT('Ctrl Pts',(-3.87500000000011,-6.71169687932933,1.59062243825055));
#8241=CARTESIAN_POINT('Ctrl Pts',(-2.49748056064562,-7.50700809845463,1.59062243825063));
#8242=CARTESIAN_POINT('Ctrl Pts',(-2.49748056064553,-7.50700809845463,8.97250262977289E-14));
#8243=CARTESIAN_POINT('Ctrl Pts',(-2.49748056064545,-7.50700809845463,-1.59062243825045));
#8244=CARTESIAN_POINT('Ctrl Pts',(-3.87499999999994,-6.71169687932933,-1.59062243825052));
#8245=CARTESIAN_POINT('Ctrl Pts',(-5.25251943935443,-5.91638566020402,-1.5906224382506));
#8246=CARTESIAN_POINT('Ctrl Pts',(-5.25251943935451,-5.91638566020402,-5.83431005538033E-14));
#8247=CARTESIAN_POINT('Ctrl Pts',(-5.2525194393546,-5.91638566020402,1.59062243825048));
#8248=CARTESIAN_POINT('Ctrl Pts',(-3.87500000000011,-6.71169687932933,1.59062243825055));
#8249=CARTESIAN_POINT('',(-3.87500000000006,-6.71169687932937,1.59062243825056));
#8250=CARTESIAN_POINT('Origin',(-3.87500000000006,-6.71169687932937,2.6565706190265E-15));
#8251=CARTESIAN_POINT('',(-4.37500000000006,-7.5777222831138,1.59062243825056));
#8252=CARTESIAN_POINT('Origin',(-4.12500000000007,-7.14470958122158,0.261524741817216));
#8253=CARTESIAN_POINT('Origin',(-4.37500000000006,-7.5777222831138,2.99935392470734E-15));
#8254=CARTESIAN_POINT('Origin',(-4.12500000000006,-7.14470958122159,-2.70146880780916E-15));
#8255=CARTESIAN_POINT('',(-2.8304244224744,-7.89213313939236,-2.05482430868446E-15));
#8256=CARTESIAN_POINT('',(-5.41957557752572,-6.39728602305082,-3.16504733330963E-15));
#8257=CARTESIAN_POINT('Origin',(-4.12500000000006,-7.14470958122159,-2.70146880780916E-15));
#8258=CARTESIAN_POINT('',(-3.87500000000006,-6.71169687932937,-1.40874692590067));
#8259=CARTESIAN_POINT('Origin',(-3.87500000000006,-6.71169687932937,2.6565706190265E-15));
#8260=CARTESIAN_POINT('',(-4.37500000000006,-7.5777222831138,-1.40874692590067));
#8261=CARTESIAN_POINT('Origin',(-4.37500000000006,-7.5777222831138,2.99935392470734E-15));
#8262=CARTESIAN_POINT('Origin',(-4.37500000000006,-7.5777222831138,-1.40874692590067));
#8263=CARTESIAN_POINT('Origin',(-3.87500000000006,-6.71169687932937,-1.59062243825055));
#8264=CARTESIAN_POINT('Ctrl Pts',(-7.57772228311387,-4.37499999999996,1.59062243825055));
#8265=CARTESIAN_POINT('Ctrl Pts',(-6.78241106398862,-5.75251943935447,1.59062243825052));
#8266=CARTESIAN_POINT('Ctrl Pts',(-6.78241106398868,-5.75251943935447,-1.35911445937371E-14));
#8267=CARTESIAN_POINT('Ctrl Pts',(-6.78241106398875,-5.75251943935447,-1.59062243825055));
#8268=CARTESIAN_POINT('Ctrl Pts',(-7.577722283114,-4.37499999999996,-1.59062243825051));
#8269=CARTESIAN_POINT('Ctrl Pts',(-8.37303350223925,-2.99748056064545,-1.59062243825048));
#8270=CARTESIAN_POINT('Ctrl Pts',(-8.37303350223919,-2.99748056064545,5.28734952023379E-14));
#8271=CARTESIAN_POINT('Ctrl Pts',(-8.37303350223912,-2.99748056064545,1.59062243825059));
#8272=CARTESIAN_POINT('Ctrl Pts',(-7.57772228311387,-4.37499999999996,1.59062243825055));
#8273=CARTESIAN_POINT('Ctrl Pts',(-7.14470958122159,-4.12499999999993,1.77871997289449));
#8274=CARTESIAN_POINT('Ctrl Pts',(-6.25534959477436,-5.66541668274533,1.77871997289445));
#8275=CARTESIAN_POINT('Ctrl Pts',(-6.25534959477443,-5.66541668274533,-3.59037940510415E-14));
#8276=CARTESIAN_POINT('Ctrl Pts',(-6.25534959477451,-5.66541668274533,-1.77871997289452));
#8277=CARTESIAN_POINT('Ctrl Pts',(-7.14470958122174,-4.12499999999993,-1.77871997289448));
#8278=CARTESIAN_POINT('Ctrl Pts',(-8.03406956766896,-2.58458331725453,-1.77871997289444));
#8279=CARTESIAN_POINT('Ctrl Pts',(-8.03406956766889,-2.58458331725453,3.94426299420347E-14));
#8280=CARTESIAN_POINT('Ctrl Pts',(-8.03406956766881,-2.58458331725453,1.77871997289452));
#8281=CARTESIAN_POINT('Ctrl Pts',(-7.14470958122159,-4.12499999999993,1.77871997289449));
#8282=CARTESIAN_POINT('Ctrl Pts',(-6.71169687932932,-3.87499999999991,1.59062243825052));
#8283=CARTESIAN_POINT('Ctrl Pts',(-5.91638566020407,-5.25251943935442,1.59062243825049));
#8284=CARTESIAN_POINT('Ctrl Pts',(-5.91638566020413,-5.25251943935442,-4.93346593113448E-14));
#8285=CARTESIAN_POINT('Ctrl Pts',(-5.9163856602042,-5.25251943935442,-1.59062243825059));
#8286=CARTESIAN_POINT('Ctrl Pts',(-6.71169687932945,-3.87499999999991,-1.59062243825055));
#8287=CARTESIAN_POINT('Ctrl Pts',(-7.50700809845471,-2.49748056064539,-1.59062243825052));
#8288=CARTESIAN_POINT('Ctrl Pts',(-7.50700809845464,-2.49748056064539,1.71299804847301E-14));
#8289=CARTESIAN_POINT('Ctrl Pts',(-7.50700809845458,-2.49748056064539,1.59062243825055));
#8290=CARTESIAN_POINT('Ctrl Pts',(-6.71169687932932,-3.87499999999991,1.59062243825052));
#8291=CARTESIAN_POINT('',(-6.71169687932944,-3.87499999999994,1.59062243825056));
#8292=CARTESIAN_POINT('Origin',(-6.71169687932943,-3.87499999999994,2.13547785601319E-15));
#8293=CARTESIAN_POINT('',(-7.57772228311388,-4.37499999999993,1.59062243825056));
#8294=CARTESIAN_POINT('Origin',(-7.14470958122164,-4.12499999999993,0.261524741817217));
#8295=CARTESIAN_POINT('Origin',(-7.57772228311388,-4.37499999999993,2.41102338582134E-15));
#8296=CARTESIAN_POINT('Origin',(-7.14470958122166,-4.12499999999993,-3.25618045875881E-15));
#8297=CARTESIAN_POINT('',(-6.39728602305091,-5.41957557752561,-3.1646474719467E-15));
#8298=CARTESIAN_POINT('',(-7.89213313939241,-2.83042442247425,-3.1646474719467E-15));
#8299=CARTESIAN_POINT('Origin',(-7.14470958122166,-4.12499999999993,-3.25618045875881E-15));
#8300=CARTESIAN_POINT('',(-6.71169687932943,-3.87499999999994,-1.40874692590067));
#8301=CARTESIAN_POINT('Origin',(-6.71169687932943,-3.87499999999994,2.13547785601319E-15));
#8302=CARTESIAN_POINT('',(-7.57772228311388,-4.37499999999993,-1.40874692590067));
#8303=CARTESIAN_POINT('Origin',(-7.57772228311388,-4.37499999999993,2.41102338582134E-15));
#8304=CARTESIAN_POINT('Origin',(-7.57772228311388,-4.37499999999993,-1.40874692590067));
#8305=CARTESIAN_POINT('Origin',(-6.71169687932943,-3.87499999999994,-1.59062243825055));
#8306=CARTESIAN_POINT('Ctrl Pts',(-8.75000000000024,8.99419774478253E-14,
1.59062243825048));
#8307=CARTESIAN_POINT('Ctrl Pts',(-8.75000000000025,-1.59062243825042,1.59062243825048));
#8308=CARTESIAN_POINT('Ctrl Pts',(-8.75000000000013,-1.59062243825043,-3.5209082131642E-14));
#8309=CARTESIAN_POINT('Ctrl Pts',(-8.75000000000001,-1.59062243825042,-1.59062243825055));
#8310=CARTESIAN_POINT('Ctrl Pts',(-8.75,8.99419774478253E-14,-1.59062243825055));
#8311=CARTESIAN_POINT('Ctrl Pts',(-8.75,1.5906224382506,-1.59062243825055));
#8312=CARTESIAN_POINT('Ctrl Pts',(-8.75000000000012,1.5906224382506,-3.52090821316413E-14));
#8313=CARTESIAN_POINT('Ctrl Pts',(-8.75000000000024,1.5906224382506,1.59062243825048));
#8314=CARTESIAN_POINT('Ctrl Pts',(-8.75000000000024,8.99419774478253E-14,
1.59062243825048));
#8315=CARTESIAN_POINT('Ctrl Pts',(-8.25000000000013,8.83781979890697E-14,
1.77871997289451));
#8316=CARTESIAN_POINT('Ctrl Pts',(-8.25000000000014,-1.77871997289442,1.77871997289451));
#8317=CARTESIAN_POINT('Ctrl Pts',(-8.25000000000001,-1.77871997289442,2.65412691824407E-15));
#8318=CARTESIAN_POINT('Ctrl Pts',(-8.24999999999987,-1.77871997289442,-1.77871997289451));
#8319=CARTESIAN_POINT('Ctrl Pts',(-8.24999999999986,8.83781979890697E-14,
-1.77871997289451));
#8320=CARTESIAN_POINT('Ctrl Pts',(-8.24999999999986,1.7787199728946,-1.77871997289451));
#8321=CARTESIAN_POINT('Ctrl Pts',(-8.24999999999999,1.7787199728946,2.65412691824491E-15));
#8322=CARTESIAN_POINT('Ctrl Pts',(-8.25000000000013,1.7787199728946,1.77871997289451));
#8323=CARTESIAN_POINT('Ctrl Pts',(-8.25000000000013,8.83781979890697E-14,
1.77871997289451));
#8324=CARTESIAN_POINT('Ctrl Pts',(-7.74999999999999,8.6814418530314E-14,
1.59062243825055));
#8325=CARTESIAN_POINT('Ctrl Pts',(-7.75,-1.59062243825043,1.59062243825055));
#8326=CARTESIAN_POINT('Ctrl Pts',(-7.74999999999988,-1.59062243825043,4.05173359681304E-14));
#8327=CARTESIAN_POINT('Ctrl Pts',(-7.74999999999976,-1.59062243825043,-1.59062243825047));
#8328=CARTESIAN_POINT('Ctrl Pts',(-7.74999999999975,8.6814418530314E-14,
-1.59062243825047));
#8329=CARTESIAN_POINT('Ctrl Pts',(-7.74999999999975,1.5906224382506,-1.59062243825047));
#8330=CARTESIAN_POINT('Ctrl Pts',(-7.74999999999987,1.5906224382506,4.05173359681311E-14));
#8331=CARTESIAN_POINT('Ctrl Pts',(-7.74999999999999,1.5906224382506,1.59062243825055));
#8332=CARTESIAN_POINT('Ctrl Pts',(-7.74999999999999,8.6814418530314E-14,
1.59062243825055));
#8333=CARTESIAN_POINT('',(-7.75,8.12743386619856E-14,1.59062243825056));
#8334=CARTESIAN_POINT('Origin',(-7.75,8.11769411281028E-14,1.42365190400878E-15));
#8335=CARTESIAN_POINT('',(-8.75,9.1748782678515E-14,1.59062243825056));
#8336=CARTESIAN_POINT('Origin',(-8.25000000000002,8.83461704452732E-14,
0.261524741817187));
#8337=CARTESIAN_POINT('Origin',(-8.75,9.16513851446323E-14,1.60734892388089E-15));
#8338=CARTESIAN_POINT('Origin',(-8.25,8.64141631363676E-14,-4.01393066573124E-15));
#8339=CARTESIAN_POINT('',(-8.25000000000002,-1.49484711634143,-3.55626573167068E-15));
#8340=CARTESIAN_POINT('',(-8.24999999999999,1.49484711634161,-4.28852962616757E-15));
#8341=CARTESIAN_POINT('Origin',(-8.25,8.64141631363676E-14,-4.01393066573124E-15));
#8342=CARTESIAN_POINT('',(-7.75,8.09181585160609E-14,-1.40874692590067));
#8343=CARTESIAN_POINT('Origin',(-7.75,8.11769411281028E-14,1.42365190400878E-15));
#8344=CARTESIAN_POINT('',(-8.75,9.13926025325903E-14,-1.40874692590067));
#8345=CARTESIAN_POINT('Origin',(-8.75,9.16513851446323E-14,1.60734892388089E-15));
#8346=CARTESIAN_POINT('Origin',(-8.75,9.13926025325903E-14,-1.40874692590067));
#8347=CARTESIAN_POINT('Origin',(-7.75,8.08847485264545E-14,-1.59062243825056));
#8348=CARTESIAN_POINT('Origin',(0.,0.,-0.416666666666667));
#8349=CARTESIAN_POINT('',(8.25,-1.01033360929657E-15,0.416666666666667));
#8350=CARTESIAN_POINT('Origin',(0.,0.,0.416666666666667));
#8351=CARTESIAN_POINT('',(8.25,-1.01033360929657E-15,-0.416666666666667));
#8352=CARTESIAN_POINT('',(8.25,-1.01033360929657E-15,-0.416666666666667));
#8353=CARTESIAN_POINT('Origin',(0.,0.,-0.416666666666667));
#8354=CARTESIAN_POINT('Origin',(0.,0.,-0.416666666666667));
#8355=CARTESIAN_POINT('',(8.75,-1.07156594925393E-15,-0.416666666666667));
#8356=CARTESIAN_POINT('Origin',(0.,0.,-0.416666666666667));
#8357=CARTESIAN_POINT('',(8.75,-1.07156594925393E-15,0.416666666666667));
#8358=CARTESIAN_POINT('',(8.75,-1.07156594925393E-15,-0.416666666666667));
#8359=CARTESIAN_POINT('Origin',(0.,0.,0.416666666666667));
#8360=CARTESIAN_POINT('Origin',(0.,0.,-0.416666666666667));
#8361=CARTESIAN_POINT('Origin',(0.,0.,0.416666666666667));
#8362=CARTESIAN_POINT('Ctrl Pts',(-7.57772228311383,4.3750000000001,1.59062243825054));
#8363=CARTESIAN_POINT('Ctrl Pts',(-8.37303350223909,2.99748056064557,1.59062243825054));
#8364=CARTESIAN_POINT('Ctrl Pts',(-8.37303350223909,2.99748056064557,-2.37492204981212E-15));
#8365=CARTESIAN_POINT('Ctrl Pts',(-8.37303350223908,2.99748056064557,-1.59062243825055));
#8366=CARTESIAN_POINT('Ctrl Pts',(-7.57772228311383,4.3750000000001,-1.59062243825055));
#8367=CARTESIAN_POINT('Ctrl Pts',(-6.78241106398857,5.75251943935462,-1.59062243825054));
#8368=CARTESIAN_POINT('Ctrl Pts',(-6.78241106398857,5.75251943935462,-1.54476000561847E-16));
#8369=CARTESIAN_POINT('Ctrl Pts',(-6.78241106398857,5.75251943935462,1.59062243825054));
#8370=CARTESIAN_POINT('Ctrl Pts',(-7.57772228311383,4.3750000000001,1.59062243825054));
#8371=CARTESIAN_POINT('Ctrl Pts',(-7.14470958122158,4.12500000000008,1.77871997289448));
#8372=CARTESIAN_POINT('Ctrl Pts',(-8.0340695676688,2.58458331725469,1.77871997289448));
#8373=CARTESIAN_POINT('Ctrl Pts',(-8.0340695676688,2.58458331725469,-1.77809156287621E-15));
#8374=CARTESIAN_POINT('Ctrl Pts',(-8.03406956766879,2.58458331725469,-1.77871997289448));
#8375=CARTESIAN_POINT('Ctrl Pts',(-7.14470958122157,4.12500000000008,-1.77871997289448));
#8376=CARTESIAN_POINT('Ctrl Pts',(-6.25534959477435,5.66541668274548,-1.77871997289448));
#8377=CARTESIAN_POINT('Ctrl Pts',(-6.25534959477435,5.66541668274548,4.42354486374065E-16));
#8378=CARTESIAN_POINT('Ctrl Pts',(-6.25534959477435,5.66541668274548,1.77871997289448));
#8379=CARTESIAN_POINT('Ctrl Pts',(-7.14470958122158,4.12500000000008,1.77871997289448));
#8380=CARTESIAN_POINT('Ctrl Pts',(-6.71169687932932,3.87500000000007,1.59062243825054));
#8381=CARTESIAN_POINT('Ctrl Pts',(-7.50700809845458,2.49748056064554,1.59062243825054));
#8382=CARTESIAN_POINT('Ctrl Pts',(-7.50700809845458,2.49748056064554,-1.18126107594029E-15));
#8383=CARTESIAN_POINT('Ctrl Pts',(-7.50700809845457,2.49748056064554,-1.59062243825054));
#8384=CARTESIAN_POINT('Ctrl Pts',(-6.71169687932932,3.87500000000007,-1.59062243825054));
#8385=CARTESIAN_POINT('Ctrl Pts',(-5.91638566020406,5.25251943935459,-1.59062243825054));
#8386=CARTESIAN_POINT('Ctrl Pts',(-5.91638566020406,5.25251943935459,1.03918497330998E-15));
#8387=CARTESIAN_POINT('Ctrl Pts',(-5.91638566020406,5.25251943935459,1.59062243825054));
#8388=CARTESIAN_POINT('Ctrl Pts',(-6.71169687932932,3.87500000000007,1.59062243825054));
#8389=CARTESIAN_POINT('',(-6.71169687932935,3.87500000000008,1.59062243825056));
#8390=CARTESIAN_POINT('Origin',(-6.71169687932935,3.87500000000008,7.11825952004385E-16));
#8391=CARTESIAN_POINT('',(-7.57772228311379,4.37500000000009,1.59062243825056));
#8392=CARTESIAN_POINT('Origin',(-7.14470958122157,4.12500000000008,0.261524741817234));
#8393=CARTESIAN_POINT('Origin',(-7.57772228311379,4.37500000000009,8.03674461940435E-16));
#8394=CARTESIAN_POINT('Origin',(-7.14470958122157,4.12500000000008,-4.77168087270366E-15));
#8395=CARTESIAN_POINT('',(-7.89213313939235,2.83042442247442,-4.68014788589155E-15));
#8396=CARTESIAN_POINT('',(-6.3972860230508,5.41957557752574,-4.68014788589155E-15));
#8397=CARTESIAN_POINT('Origin',(-7.14470958122157,4.12500000000008,-4.77168087270366E-15));
#8398=CARTESIAN_POINT('',(-6.71169687932935,3.87500000000008,-1.40874692590067));
#8399=CARTESIAN_POINT('Origin',(-6.71169687932935,3.87500000000008,7.11825952004385E-16));
#8400=CARTESIAN_POINT('',(-7.57772228311379,4.37500000000009,-1.40874692590067));
#8401=CARTESIAN_POINT('Origin',(-7.57772228311379,4.37500000000009,8.03674461940435E-16));
#8402=CARTESIAN_POINT('Origin',(-7.57772228311379,4.37500000000009,-1.40874692590067));
#8403=CARTESIAN_POINT('Origin',(-6.71169687932935,3.87500000000008,-1.59062243825056));
#8404=CARTESIAN_POINT('Ctrl Pts',(-4.3749999999999,7.5777222831139,1.59062243825056));
#8405=CARTESIAN_POINT('Ctrl Pts',(-5.75251943935444,6.78241106398865,1.59062243825055));
#8406=CARTESIAN_POINT('Ctrl Pts',(-5.75251943935444,6.78241106398865,1.08090394793333E-15));
#8407=CARTESIAN_POINT('Ctrl Pts',(-5.75251943935444,6.78241106398866,-1.59062243825055));
#8408=CARTESIAN_POINT('Ctrl Pts',(-4.3749999999999,7.5777222831139,-1.59062243825055));
#8409=CARTESIAN_POINT('Ctrl Pts',(-2.99748056064537,8.37303350223915,-1.59062243825055));
#8410=CARTESIAN_POINT('Ctrl Pts',(-2.99748056064537,8.37303350223915,5.5217960464338E-15));
#8411=CARTESIAN_POINT('Ctrl Pts',(-2.99748056064537,8.37303350223915,1.59062243825056));
#8412=CARTESIAN_POINT('Ctrl Pts',(-4.3749999999999,7.5777222831139,1.59062243825056));
#8413=CARTESIAN_POINT('Ctrl Pts',(-4.12499999999991,7.14470958122166,1.77871997289447));
#8414=CARTESIAN_POINT('Ctrl Pts',(-5.6654166827453,6.25534959477446,1.77871997289446));
#8415=CARTESIAN_POINT('Ctrl Pts',(-5.6654166827453,6.25534959477447,-1.12757025938426E-16));
#8416=CARTESIAN_POINT('Ctrl Pts',(-5.6654166827453,6.25534959477447,-1.77871997289446));
#8417=CARTESIAN_POINT('Ctrl Pts',(-4.12499999999991,7.14470958122167,-1.77871997289446));
#8418=CARTESIAN_POINT('Ctrl Pts',(-2.58458331725452,8.03406956766888,-1.77871997289446));
#8419=CARTESIAN_POINT('Ctrl Pts',(-2.58458331725452,8.03406956766887,4.32813507256205E-15));
#8420=CARTESIAN_POINT('Ctrl Pts',(-2.58458331725452,8.03406956766887,1.77871997289447));
#8421=CARTESIAN_POINT('Ctrl Pts',(-4.12499999999991,7.14470958122166,1.77871997289447));
#8422=CARTESIAN_POINT('Ctrl Pts',(-3.87499999999991,6.71169687932943,1.59062243825055));
#8423=CARTESIAN_POINT('Ctrl Pts',(-5.25251943935445,5.91638566020418,1.59062243825055));
#8424=CARTESIAN_POINT('Ctrl Pts',(-5.25251943935445,5.91638566020419,-8.25677328214282E-16));
#8425=CARTESIAN_POINT('Ctrl Pts',(-5.25251943935445,5.91638566020419,-1.59062243825055));
#8426=CARTESIAN_POINT('Ctrl Pts',(-3.87499999999991,6.71169687932944,-1.59062243825055));
#8427=CARTESIAN_POINT('Ctrl Pts',(-2.49748056064538,7.50700809845469,-1.59062243825055));
#8428=CARTESIAN_POINT('Ctrl Pts',(-2.49748056064537,7.50700809845469,2.6537334270944E-15));
#8429=CARTESIAN_POINT('Ctrl Pts',(-2.49748056064537,7.50700809845468,1.59062243825055));
#8430=CARTESIAN_POINT('Ctrl Pts',(-3.87499999999991,6.71169687932943,1.59062243825055));
#8431=CARTESIAN_POINT('',(-3.87499999999991,6.71169687932945,1.59062243825056));
#8432=CARTESIAN_POINT('Origin',(-3.87499999999991,6.71169687932945,1.90733188991085E-16));
#8433=CARTESIAN_POINT('',(-4.3749999999999,7.57772228311389,1.59062243825056));
#8434=CARTESIAN_POINT('Origin',(-4.12499999999991,7.14470958122167,0.26152474181723));
#8435=CARTESIAN_POINT('Origin',(-4.3749999999999,7.57772228311389,2.15343923054451E-16));
#8436=CARTESIAN_POINT('Origin',(-4.12499999999991,7.14470958122167,-5.32639252365331E-15));
#8437=CARTESIAN_POINT('',(-5.41957557752559,6.39728602305093,-5.2348595368412E-15));
#8438=CARTESIAN_POINT('',(-2.83042442247423,7.89213313939241,-5.2348595368412E-15));
#8439=CARTESIAN_POINT('Origin',(-4.12499999999991,7.14470958122167,-5.32639252365331E-15));
#8440=CARTESIAN_POINT('',(-3.87499999999991,6.71169687932945,-1.40874692590067));
#8441=CARTESIAN_POINT('Origin',(-3.87499999999991,6.71169687932945,1.90733188991085E-16));
#8442=CARTESIAN_POINT('',(-4.3749999999999,7.5777222831139,-1.40874692590067));
#8443=CARTESIAN_POINT('Origin',(-4.3749999999999,7.57772228311389,2.15343923054451E-16));
#8444=CARTESIAN_POINT('Origin',(-4.3749999999999,7.57772228311389,-1.40874692590067));
#8445=CARTESIAN_POINT('Origin',(-3.87499999999991,6.71169687932945,-1.59062243825056));
#8446=CARTESIAN_POINT('Origin',(-7.14470958122157,4.12500000000008,7.5775020697241E-16));
#8447=CARTESIAN_POINT('',(-7.89213313939235,2.83042442247441,9.95559882563082E-16));
#8448=CARTESIAN_POINT('',(-6.39728602305079,5.41957557752575,5.19940531381738E-16));
#8449=CARTESIAN_POINT('Origin',(-7.14470958122157,4.12500000000008,7.5775020697241E-16));
#8450=CARTESIAN_POINT('Origin',(-4.12499999999991,7.14470958122167,2.03038556022768E-16));
#8451=CARTESIAN_POINT('',(-5.4195755775256,6.39728602305092,3.40338036240938E-16));
#8452=CARTESIAN_POINT('',(-2.83042442247422,7.89213313939242,6.5739075804598E-17));
#8453=CARTESIAN_POINT('Origin',(-4.12499999999991,7.14470958122167,2.03038556022768E-16));
#8454=CARTESIAN_POINT('Origin',(0.,5.1026949964479E-18,-2.47222222222222));
#8455=CARTESIAN_POINT('',(-9.09640428033339E-16,-7.42777777777777,-2.5));
#8456=CARTESIAN_POINT('Origin',(0.,6.13137853388905E-31,-2.5));
#8457=CARTESIAN_POINT('',(9.0623863136904E-16,-7.39999999999999,-2.47222222222222));
#8458=CARTESIAN_POINT('Origin',(9.09640428033339E-16,-7.42777777777777,
-2.47222222222222));
#8459=CARTESIAN_POINT('',(9.06238631369041E-16,7.39999999999999,-2.47222222222222));
#8460=CARTESIAN_POINT('Origin',(0.,5.1026949964479E-18,-2.47222222222222));
#8461=CARTESIAN_POINT('Origin',(0.,5.1026949964479E-18,-2.47222222222222));
#8462=CARTESIAN_POINT('Origin',(0.,5.1026949964479E-18,-2.47222222222222));
#8463=CARTESIAN_POINT('',(1.11442858722409E-15,9.1,-2.47222222222222));
#8464=CARTESIAN_POINT('',(1.11442858722409E-15,-9.1,-2.47222222222222));
#8465=CARTESIAN_POINT('Origin',(0.,5.10269499644792E-18,-2.47222222222222));
#8466=CARTESIAN_POINT('',(-1.11102679055979E-15,-9.07222222222223,-2.5));
#8467=CARTESIAN_POINT('Origin',(1.11102679055979E-15,-9.07222222222223,
-2.47222222222222));
#8468=CARTESIAN_POINT('Origin',(0.,6.13137853388905E-31,-2.5));
#8469=CARTESIAN_POINT('Origin',(0.,5.10269499644792E-18,-2.47222222222222));
#8470=CARTESIAN_POINT('Origin',(0.,0.,-2.5));
#8471=CARTESIAN_POINT('',(1.1236134382177E-15,-9.1,-2.31481481481481));
#8472=CARTESIAN_POINT('',(-1.11442858722409E-15,9.1,-2.31481481481481));
#8473=CARTESIAN_POINT('Origin',(0.,3.40179666429828E-17,-2.31481481481481));
#8474=CARTESIAN_POINT('Origin',(0.,3.40179666429828E-17,-2.31481481481481));
#8475=CARTESIAN_POINT('',(-1.11442858722409E-15,9.1,-2.5));
#8476=CARTESIAN_POINT('Origin',(0.,5.10269499644737E-17,-2.22222222222222));
#8477=CARTESIAN_POINT('',(-1.1327982892113E-15,-9.25000000000001,-2.22222222222222));
#8478=CARTESIAN_POINT('Origin',(0.,5.10269499644737E-17,-2.22222222222222));
#8479=CARTESIAN_POINT('',(1.1327982892113E-15,-9.25000000000001,-2.22222222222222));
#8480=CARTESIAN_POINT('Origin',(0.,3.40179666429827E-17,-2.31481481481481));
#8481=CARTESIAN_POINT('',(-8.8786892938183E-16,7.24999999999999,-2.22222222222222));
#8482=CARTESIAN_POINT('Origin',(0.,5.10269499644738E-17,-2.22222222222222));
#8483=CARTESIAN_POINT('',(-9.06238631369041E-16,7.39999999999999,-2.31481481481481));
#8484=CARTESIAN_POINT('',(9.0623863136904E-16,7.39999999999999,-2.31481481481481));
#8485=CARTESIAN_POINT('Origin',(0.,3.40179666429827E-17,-2.31481481481481));
#8486=CARTESIAN_POINT('Origin',(0.,0.,-2.5));
#8487=CARTESIAN_POINT('',(-9.0623863136904E-16,7.39999999999999,-2.5));
#8488=CARTESIAN_POINT('Origin',(0.,9.1,-2.5));
#8489=CARTESIAN_POINT('Origin',(0.,9.25000000000001,-2.22222222222222));
#8490=CARTESIAN_POINT('Origin',(0.,9.13382404364069E-16,2.47222222222223));
#8491=CARTESIAN_POINT('',(-1.11442858722409E-15,9.1,2.47222222222223));
#8492=CARTESIAN_POINT('Origin',(0.,9.13382404364069E-16,2.47222222222223));
#8493=CARTESIAN_POINT('',(-1.11102679055979E-15,9.07222222222223,2.50000000000001));
#8494=CARTESIAN_POINT('Origin',(1.11102679055979E-15,9.07222222222222,2.47222222222223));
#8495=CARTESIAN_POINT('Origin',(0.,9.18485099360517E-16,2.50000000000001));
#8496=CARTESIAN_POINT('Origin',(0.,9.13382404364069E-16,2.47222222222223));
#8497=CARTESIAN_POINT('',(-9.09640428033339E-16,7.42777777777777,2.50000000000001));
#8498=CARTESIAN_POINT('Origin',(0.,9.18485099360517E-16,2.50000000000001));
#8499=CARTESIAN_POINT('',(-9.06238631369041E-16,7.39999999999999,2.47222222222223));
#8500=CARTESIAN_POINT('Origin',(9.09640428033339E-16,7.42777777777777,2.47222222222223));
#8501=CARTESIAN_POINT('Origin',(0.,9.13382404364069E-16,2.47222222222223));
#8502=CARTESIAN_POINT('Origin',(0.,0.,-2.5));
#8503=CARTESIAN_POINT('',(9.06238631369041E-16,-7.39999999999999,2.31481481481482));
#8504=CARTESIAN_POINT('',(-9.0623863136904E-16,7.39999999999999,2.31481481481482));
#8505=CARTESIAN_POINT('Origin',(0.,8.84467132717534E-16,2.31481481481482));
#8506=CARTESIAN_POINT('Origin',(0.,8.84467132717534E-16,2.31481481481482));
#8507=CARTESIAN_POINT('',(-9.0623863136904E-16,7.39999999999999,-2.5));
#8508=CARTESIAN_POINT('Origin',(0.,8.67458149396043E-16,2.22222222222223));
#8509=CARTESIAN_POINT('',(-8.8786892938183E-16,-7.24999999999999,2.22222222222223));
#8510=CARTESIAN_POINT('Origin',(0.,8.67458149396043E-16,2.22222222222223));
#8511=CARTESIAN_POINT('',(8.8786892938183E-16,-7.24999999999999,2.22222222222223));
#8512=CARTESIAN_POINT('Origin',(0.,8.84467132717534E-16,2.31481481481482));
#8513=CARTESIAN_POINT('',(-1.1327982892113E-15,9.25000000000001,2.22222222222223));
#8514=CARTESIAN_POINT('Origin',(0.,8.67458149396044E-16,2.22222222222223));
#8515=CARTESIAN_POINT('',(-1.11442858722409E-15,9.1,2.31481481481482));
#8516=CARTESIAN_POINT('',(1.11442858722409E-15,9.1,2.31481481481482));
#8517=CARTESIAN_POINT('Origin',(0.,8.84467132717534E-16,2.31481481481482));
#8518=CARTESIAN_POINT('Origin',(0.,0.,-2.5));
#8519=CARTESIAN_POINT('',(-1.11442858722409E-15,9.1,-2.5));
#8520=CARTESIAN_POINT('Origin',(0.,7.24999999999999,2.22222222222223));
#8521=CARTESIAN_POINT('Origin',(0.,9.1,2.50000000000001));
#8522=CARTESIAN_POINT('',(0.,0.,0.));
#8523=CARTESIAN_POINT('Origin',(0.,0.,-15.693275));
#8524=CARTESIAN_POINT('',(2.94200000000002,3.60291088309151E-16,-15.4940369700794));
#8525=CARTESIAN_POINT('Origin',(1.58481671019917E-14,0.,-15.4940369700794));
#8526=CARTESIAN_POINT('',(2.38654999999999,-2.9226808185051E-16,-16.));
#8527=CARTESIAN_POINT('',(2.72327499999996,3.33505001194796E-16,-15.693275));
#8528=CARTESIAN_POINT('Origin',(0.,0.,-16.));
#8529=CARTESIAN_POINT('Origin',(-3.26269418602128E-14,0.,5.39999999999958));
#8530=CARTESIAN_POINT('',(4.99999999999974,-6.12323399573649E-16,5.39999999999959));
#8531=CARTESIAN_POINT('Origin',(-3.26269418602128E-14,0.,5.39999999999958));
#8532=CARTESIAN_POINT('',(4.39999999999974,-5.38844591624807E-16,5.99999999999959));
#8533=CARTESIAN_POINT('Origin',(4.39999999999974,-5.38844591624807E-16,
5.39999999999959));
#8534=CARTESIAN_POINT('Origin',(-3.40189689452119E-14,0.,5.99999999999958));
#8535=CARTESIAN_POINT('Origin',(-4.9999999999998,0.,5.99999999999957));
#8536=CARTESIAN_POINT('',(2.5,-1.44337567297406,6.));
#8537=CARTESIAN_POINT('',(0.,-2.88675134594813,6.));
#8538=CARTESIAN_POINT('',(7.46624984060421E-14,-2.88675134594809,5.99999999999958));
#8539=CARTESIAN_POINT('',(-2.5,-1.44337567297406,6.));
#8540=CARTESIAN_POINT('',(-2.49999999999993,-1.44337567297411,5.99999999999957));
#8541=CARTESIAN_POINT('',(-2.5,1.44337567297407,6.));
#8542=CARTESIAN_POINT('',(-2.5,-0.721687836487033,5.99999999999957));
#8543=CARTESIAN_POINT('',(3.64291929955129E-16,2.88675134594813,6.));
#8544=CARTESIAN_POINT('',(-3.74999999999992,0.721687836487077,5.99999999999957));
#8545=CARTESIAN_POINT('',(2.5,1.44337567297406,6.));
#8546=CARTESIAN_POINT('',(-1.24999999999992,3.60843918243512,5.99999999999958));
#8547=CARTESIAN_POINT('',(2.5,0.721687836487032,5.99999999999958));
#8548=CARTESIAN_POINT('Origin',(-2.70588335202164E-14,0.,2.99999999999958));
#8549=CARTESIAN_POINT('',(4.99999999999975,-6.12323399573649E-16,-4.10227407598995E-13));
#8550=CARTESIAN_POINT('Origin',(-2.00986980952208E-14,0.,-4.2159796951126E-13));
#8551=CARTESIAN_POINT('',(4.99999999999974,-6.12323399573649E-16,2.99999999999959));
#8552=CARTESIAN_POINT('Origin',(0.,-2.88675134594813,3.));
#8553=CARTESIAN_POINT('',(0.,-2.88675134594813,3.));
#8554=CARTESIAN_POINT('',(-1.31861671037658E-15,-5.55111512312578E-16,2.78127834118519));
#8555=CARTESIAN_POINT('',(-1.66533453693773E-15,-2.16918285467233,2.9456316973939));
#8556=CARTESIAN_POINT('',(2.5,-1.44337567297406,3.));
#8557=CARTESIAN_POINT('',(1.24247637239728E-16,-2.88675134594813,3.));
#8558=CARTESIAN_POINT('',(1.87856745759988,-1.08459142733617,2.9456316973939));
#8559=CARTESIAN_POINT('Origin',(2.5,-1.44337567297406,3.));
#8560=CARTESIAN_POINT('',(2.5,1.44337567297406,3.));
#8561=CARTESIAN_POINT('',(2.5,-1.44337567297406,3.));
#8562=CARTESIAN_POINT('',(1.87856745759989,1.08459142733616,2.9456316973939));
#8563=CARTESIAN_POINT('Origin',(2.5,1.44337567297406,3.));
#8564=CARTESIAN_POINT('',(5.55111512312578E-16,2.88675134594813,3.));
#8565=CARTESIAN_POINT('',(2.5,1.44337567297406,3.));
#8566=CARTESIAN_POINT('',(1.38777878078145E-15,2.16918285467233,2.9456316973939));
#8567=CARTESIAN_POINT('Origin',(5.55111512312578E-16,2.88675134594813,3.));
#8568=CARTESIAN_POINT('',(-2.5,1.44337567297407,3.));
#8569=CARTESIAN_POINT('',(3.64291929955129E-16,2.88675134594813,3.));
#8570=CARTESIAN_POINT('',(-1.87856745759989,1.08459142733617,2.9456316973939));
#8571=CARTESIAN_POINT('Origin',(-2.5,1.44337567297407,3.));
#8572=CARTESIAN_POINT('',(-2.5,-1.44337567297406,3.));
#8573=CARTESIAN_POINT('',(-2.5,1.44337567297407,3.));
#8574=CARTESIAN_POINT('',(-1.87856745759989,-1.08459142733616,2.9456316973939));
#8575=CARTESIAN_POINT('Origin',(-2.5,-1.44337567297406,3.));
#8576=CARTESIAN_POINT('',(-2.5,-1.44337567297406,3.));
#8577=CARTESIAN_POINT('Origin',(2.5,-1.44337567297406,6.));
#8578=CARTESIAN_POINT('',(2.5,-1.44337567297406,6.));
#8579=CARTESIAN_POINT('',(0.,-2.88675134594813,6.));
#8580=CARTESIAN_POINT('Origin',(2.5,1.44337567297406,6.));
#8581=CARTESIAN_POINT('',(2.5,1.44337567297406,6.));
#8582=CARTESIAN_POINT('Origin',(0.,2.88675134594813,6.));
#8583=CARTESIAN_POINT('',(3.64291929955129E-16,2.88675134594813,6.));
#8584=CARTESIAN_POINT('Origin',(-2.5,1.44337567297407,6.));
#8585=CARTESIAN_POINT('',(-2.5,1.44337567297407,6.));
#8586=CARTESIAN_POINT('Origin',(-2.5,-1.44337567297406,6.));
#8587=CARTESIAN_POINT('',(-2.5,-1.44337567297406,6.));
#8588=CARTESIAN_POINT('Origin',(0.,-2.88675134594813,6.));
#8589=CARTESIAN_POINT('Origin',(-1.53833696190003E-15,0.,-8.00000000000013));
#8590=CARTESIAN_POINT('',(2.94199999999998,3.60291088309151E-16,-2.53037902429339E-13));
#8591=CARTESIAN_POINT('',(2.942,-3.60291088309151E-16,-8.00000000000012));
#8592=CARTESIAN_POINT('Origin',(-2.00986980952212E-14,0.,-2.59792187762287E-13));
#8593=CARTESIAN_POINT('Origin',(1.72084568816899E-14,0.,-16.));
#8594=CARTESIAN_POINT('Origin',(-2.9999999999998,0.,-2.66583504750515E-13));
#8595=CARTESIAN_POINT('',(0.,0.,0.));
#8596=CARTESIAN_POINT('Origin',(-150.,37.8343839603864,-7.99999999999999));
#8597=CARTESIAN_POINT('',(-140.,40.8343839603864,-7.99999999999999));
#8598=CARTESIAN_POINT('Origin',(-140.,37.8343839603864,-7.99999999999999));
#8599=CARTESIAN_POINT('',(-126.,40.8343839603864,-7.99999999999999));
#8600=CARTESIAN_POINT('',(-150.,40.8343839603864,-7.99999999999999));
#8601=CARTESIAN_POINT('Origin',(-126.,37.8343839603864,-7.99999999999999));
#8602=CARTESIAN_POINT('Origin',(-126.,37.8343839603864,-7.99999999999999));
#8603=CARTESIAN_POINT('Origin',(150.,37.8343839603864,-8.00000000000001));
#8604=CARTESIAN_POINT('',(140.,34.8343839603864,-8.00000000000001));
#8605=CARTESIAN_POINT('Origin',(140.,37.8343839603864,-8.00000000000001));
#8606=CARTESIAN_POINT('',(120.,34.8343839603864,-8.00000000000001));
#8607=CARTESIAN_POINT('',(150.,34.8343839603864,-8.00000000000001));
#8608=CARTESIAN_POINT('Origin',(120.,37.8343839603864,-8.00000000000001));
#8609=CARTESIAN_POINT('Origin',(120.,37.8343839603864,-8.00000000000001));
#8610=CARTESIAN_POINT('Origin',(-140.,37.8343839603864,-7.99999999999999));
#8611=CARTESIAN_POINT('',(-140.,43.8343839603864,-7.99999999999999));
#8612=CARTESIAN_POINT('Origin',(-140.,37.8343839603864,-7.99999999999999));
#8613=CARTESIAN_POINT('Origin',(0.,37.8343839603864,-7.99999999999999));
#8614=CARTESIAN_POINT('',(140.,43.8343839603864,-7.99999999999999));
#8615=CARTESIAN_POINT('',(0.,43.8343839603864,-7.99999999999999));
#8616=CARTESIAN_POINT('Origin',(140.,37.8343839603864,-7.99999999999999));
#8617=CARTESIAN_POINT('Origin',(140.,37.8343839603864,-7.99999999999999));
#8618=CARTESIAN_POINT('',(0.,0.,0.));
#8619=CARTESIAN_POINT('Origin',(-135.,2.22044604925031E-15,9.99200722162641E-15));
#8620=CARTESIAN_POINT('',(-135.,-7.50000000000001,9.6119802892091E-15));
#8621=CARTESIAN_POINT('Origin',(-135.,1.91963385766348E-15,1.05304653885696E-14));
#8622=CARTESIAN_POINT('Origin',(0.,1.91963385766348E-15,1.05304653885696E-14));
#8623=CARTESIAN_POINT('',(135.,-7.50000000000001,9.6119802892091E-15));
#8624=CARTESIAN_POINT('Origin',(135.,1.91963385766348E-15,1.05304653885696E-14));
#8625=CARTESIAN_POINT('',(0.,-7.50000000000001,9.61198028920908E-15));
#8626=CARTESIAN_POINT('Origin',(135.,2.22044604925031E-15,9.99200722162641E-15));
#8627=CARTESIAN_POINT('',(0.,0.,0.));
#8628=CARTESIAN_POINT('Origin',(-150.,-37.8343839603864,-7.99999999999999));
#8629=CARTESIAN_POINT('',(-140.,-34.8343839603864,-7.99999999999999));
#8630=CARTESIAN_POINT('Origin',(-140.,-37.8343839603864,-7.99999999999999));
#8631=CARTESIAN_POINT('',(-126.,-34.8343839603864,-7.99999999999999));
#8632=CARTESIAN_POINT('',(-150.,-34.8343839603864,-7.99999999999999));
#8633=CARTESIAN_POINT('Origin',(-126.,-37.8343839603864,-7.99999999999999));
#8634=CARTESIAN_POINT('Origin',(-126.,-37.8343839603864,-7.99999999999999));
#8635=CARTESIAN_POINT('Origin',(150.,-37.8343839603864,-8.00000000000001));
#8636=CARTESIAN_POINT('',(140.,-40.8343839603864,-8.00000000000001));
#8637=CARTESIAN_POINT('Origin',(140.,-37.8343839603864,-8.00000000000001));
#8638=CARTESIAN_POINT('',(120.,-40.8343839603864,-8.00000000000001));
#8639=CARTESIAN_POINT('',(150.,-40.8343839603864,-8.00000000000001));
#8640=CARTESIAN_POINT('Origin',(120.,-37.8343839603864,-8.00000000000001));
#8641=CARTESIAN_POINT('Origin',(120.,-37.8343839603864,-8.00000000000001));
#8642=CARTESIAN_POINT('Origin',(-140.,-37.8343839603864,-7.99999999999999));
#8643=CARTESIAN_POINT('',(-140.,-43.8343839603864,-7.99999999999999));
#8644=CARTESIAN_POINT('Origin',(-140.,-37.8343839603864,-7.99999999999999));
#8645=CARTESIAN_POINT('Origin',(0.,-37.8343839603864,-7.99999999999999));
#8646=CARTESIAN_POINT('',(140.,-43.8343839603864,-7.99999999999999));
#8647=CARTESIAN_POINT('Origin',(140.,-37.8343839603864,-7.99999999999999));
#8648=CARTESIAN_POINT('',(0.,-43.8343839603864,-7.99999999999999));
#8649=CARTESIAN_POINT('Origin',(140.,-37.8343839603864,-7.99999999999999));
#8650=CARTESIAN_POINT('',(0.,0.,0.));
#8651=CARTESIAN_POINT('Origin',(0.,1.73472347597681E-15,-2.60208521396521E-15));
#8652=CARTESIAN_POINT('',(1.34711147906209E-15,11.,2.44444444444444));
#8653=CARTESIAN_POINT('Origin',(0.,5.61296449609204E-16,2.44444444444444));
#8654=CARTESIAN_POINT('',(-1.34711147906209E-15,11.,-2.44444444444444));
#8655=CARTESIAN_POINT('Origin',(-1.53080849893419E-15,12.5,-3.05872465563923E-16));
#8656=CARTESIAN_POINT('Origin',(0.,1.45937076898393E-15,-2.44444444444445));
#8657=CARTESIAN_POINT('Origin',(0.,-6.84346607882717E-31,5.5));
#8658=CARTESIAN_POINT('',(-9.18485099360515E-16,7.5,4.95));
#8659=CARTESIAN_POINT('Origin',(0.,1.01033360929656E-16,4.95));
#8660=CARTESIAN_POINT('',(-9.85840673313618E-16,8.04999999999999,5.50000000000001));
#8661=CARTESIAN_POINT('',(-9.85840673313618E-16,8.04999999999999,5.5));
#8662=CARTESIAN_POINT('Origin',(0.,-6.84346607882717E-31,5.5));
#8663=CARTESIAN_POINT('Origin',(0.,0.,5.5));
#8664=CARTESIAN_POINT('',(9.52162886337066E-16,-7.5,-4.95000000000001));
#8665=CARTESIAN_POINT('',(-9.18485099360515E-16,7.5,-4.95000000000001));
#8666=CARTESIAN_POINT('Origin',(0.,1.91963385766348E-15,-4.95000000000001));
#8667=CARTESIAN_POINT('Origin',(0.,1.91963385766348E-15,-4.95000000000001));
#8668=CARTESIAN_POINT('',(-9.18485099360515E-16,7.5,5.5));
#8669=CARTESIAN_POINT('Origin',(0.,1.91963385766348E-15,-4.95000000000001));
#8670=CARTESIAN_POINT('',(-9.85840673313618E-16,-8.04999999999999,-5.50000000000001));
#8671=CARTESIAN_POINT('',(-9.18485099360515E-16,-7.5,-4.95000000000001));
#8672=CARTESIAN_POINT('Origin',(0.,2.02066721859313E-15,-5.50000000000001));
#8673=CARTESIAN_POINT('Origin',(0.,0.,5.5));
#8674=CARTESIAN_POINT('',(-1.34711147906209E-15,11.,-5.50000000000001));
#8675=CARTESIAN_POINT('',(-1.34711147906209E-15,11.,5.5));
#8676=CARTESIAN_POINT('Origin',(0.,2.02066721859313E-15,-5.50000000000001));
#8677=CARTESIAN_POINT('Origin',(0.,0.,5.5));
#8678=CARTESIAN_POINT('',(-1.34711147906209E-15,11.,5.50000000000001));
#8679=CARTESIAN_POINT('Origin',(0.,-9.03463585147651E-31,5.50000000000001));
#8680=CARTESIAN_POINT('',(-1.34711147906209E-15,11.,5.5));
#8681=CARTESIAN_POINT('Origin',(0.,8.04999999999999,5.50000000000001));
#8682=CARTESIAN_POINT('Origin',(0.,8.04999999999999,-5.50000000000001));
#8683=CARTESIAN_POINT('Origin',(0.,12.5,0.));
#8684=CARTESIAN_POINT('',(-2.86797988869785,12.5,2.15064044727603E-32));
#8685=CARTESIAN_POINT('',(2.86797988869785,12.5,2.15064044727603E-32));
#8686=CARTESIAN_POINT('Origin',(0.,12.5,0.));
#8687=CARTESIAN_POINT('Origin',(0.,2.02066721859313E-15,-5.50000000000001));
#8688=CARTESIAN_POINT('',(-2.14313189850787E-15,17.5,-4.95000000000001));
#8689=CARTESIAN_POINT('Origin',(0.,1.91963385766348E-15,-4.95000000000001));
#8690=CARTESIAN_POINT('',(-2.07577632455476E-15,16.95,-5.5));
#8691=CARTESIAN_POINT('',(-2.07577632455476E-15,16.95,-5.50000000000001));
#8692=CARTESIAN_POINT('Origin',(0.,2.02066721859313E-15,-5.50000000000001));
#8693=CARTESIAN_POINT('Origin',(0.,0.,5.5));
#8694=CARTESIAN_POINT('',(-1.7145055188063E-15,14.,-5.50000000000001));
#8695=CARTESIAN_POINT('Origin',(0.,2.02066721859313E-15,-5.50000000000001));
#8696=CARTESIAN_POINT('',(-1.7145055188063E-15,14.,-2.44444444444444));
#8697=CARTESIAN_POINT('',(-1.71450551880629E-15,14.,5.5));
#8698=CARTESIAN_POINT('Origin',(0.,1.45937076898393E-15,-2.44444444444445));
#8699=CARTESIAN_POINT('Origin',(0.,1.73472347597681E-15,-2.60208521396521E-15));
#8700=CARTESIAN_POINT('',(-1.7145055188063E-15,14.,2.44444444444445));
#8701=CARTESIAN_POINT('Origin',(-1.53080849893419E-15,12.5,-3.05872465563923E-16));
#8702=CARTESIAN_POINT('Origin',(0.,5.61296449609204E-16,2.44444444444444));
#8703=CARTESIAN_POINT('Origin',(0.,0.,5.5));
#8704=CARTESIAN_POINT('',(-1.7145055188063E-15,14.,5.5));
#8705=CARTESIAN_POINT('',(-1.71450551880629E-15,14.,5.5));
#8706=CARTESIAN_POINT('Origin',(0.,7.91087864377601E-31,5.5));
#8707=CARTESIAN_POINT('Origin',(0.,1.01033360929657E-16,4.94999999999999));
#8708=CARTESIAN_POINT('',(2.14313189850787E-15,17.5,4.95));
#8709=CARTESIAN_POINT('',(-2.14313189850787E-15,-17.5,4.94999999999999));
#8710=CARTESIAN_POINT('Origin',(0.,1.01033360929657E-16,4.94999999999999));
#8711=CARTESIAN_POINT('',(-2.07577632455476E-15,-16.95,5.49999999999999));
#8712=CARTESIAN_POINT('',(-2.14313189850787E-15,-17.5,4.94999999999999));
#8713=CARTESIAN_POINT('Origin',(0.,1.2092979527909E-30,5.49999999999999));
#8714=CARTESIAN_POINT('Origin',(0.,1.01033360929657E-16,4.94999999999999));
#8715=CARTESIAN_POINT('Origin',(0.,0.,5.5));
#8716=CARTESIAN_POINT('',(-2.14313189850787E-15,17.5,5.5));
#8717=CARTESIAN_POINT('Origin',(0.,16.95,5.5));
#8718=CARTESIAN_POINT('Origin',(0.,16.95,-5.5));
#8719=CARTESIAN_POINT('Origin',(8.83883476483186,8.83883476483183,-6.7254514295974E-16));
#8720=CARTESIAN_POINT('',(6.81086673722698,10.8668027924367,-3.00013459892815E-16));
#8721=CARTESIAN_POINT('',(10.8668027924367,6.81086673722694,-1.04507682602666E-15));
#8722=CARTESIAN_POINT('Origin',(8.83883476483186,8.83883476483183,-6.7254514295974E-16));
#8723=CARTESIAN_POINT('Origin',(12.5,-4.36435167355392E-14,-2.2962127484013E-15));
#8724=CARTESIAN_POINT('',(12.5,2.86797988869781,-1.76937338979438E-15));
#8725=CARTESIAN_POINT('',(12.5,-2.86797988869789,-2.82305210700822E-15));
#8726=CARTESIAN_POINT('Origin',(12.5,-4.36435167355392E-14,-2.2962127484013E-15));
#8727=CARTESIAN_POINT('Origin',(8.8388347648318,-8.83883476483189,-3.91988035384285E-15));
#8728=CARTESIAN_POINT('',(10.8668027924367,-6.81086673722701,-3.54734867077593E-15));
#8729=CARTESIAN_POINT('',(6.8108667372269,-10.8668027924368,-4.29241203690977E-15));
#8730=CARTESIAN_POINT('Origin',(8.8388347648318,-8.83883476483189,-3.91988035384285E-15));
#8731=CARTESIAN_POINT('Origin',(0.,-12.5,-4.59242549680258E-15));
#8732=CARTESIAN_POINT('',(2.86797988869785,-12.5,-4.59242549680258E-15));
#8733=CARTESIAN_POINT('',(-2.86797988869785,-12.5,-4.59242549680258E-15));
#8734=CARTESIAN_POINT('Origin',(0.,-12.5,-4.59242549680258E-15));
#8735=CARTESIAN_POINT('Origin',(-8.83883476483192,-8.83883476483177,-3.91988035384282E-15));
#8736=CARTESIAN_POINT('',(-6.81086673722705,-10.8668027924367,-4.29241203690975E-15));
#8737=CARTESIAN_POINT('',(-10.8668027924368,-6.81086673722686,-3.54734867077589E-15));
#8738=CARTESIAN_POINT('Origin',(-8.83883476483192,-8.83883476483177,-3.91988035384282E-15));
#8739=CARTESIAN_POINT('Origin',(-12.5,1.30930550206618E-13,-2.29621274840126E-15));
#8740=CARTESIAN_POINT('',(-12.5,-2.86797988869772,-2.82305210700818E-15));
#8741=CARTESIAN_POINT('',(-12.5,2.86797988869798,-1.76937338979434E-15));
#8742=CARTESIAN_POINT('Origin',(-12.5,1.30930550206618E-13,-2.29621274840126E-15));
#8743=CARTESIAN_POINT('Origin',(-8.83883476483174,8.83883476483195,-6.72545142959718E-16));
#8744=CARTESIAN_POINT('',(-10.8668027924367,6.81086673722708,-1.04507682602664E-15));
#8745=CARTESIAN_POINT('',(-6.81086673722683,10.8668027924368,-3.00013459892799E-16));
#8746=CARTESIAN_POINT('Origin',(-8.83883476483174,8.83883476483195,-6.72545142959718E-16));
#8747=CARTESIAN_POINT('Origin',(0.,12.5,0.));
#8748=CARTESIAN_POINT('',(-3.94762635814864E-16,13.25,-3.22348154659542));
#8749=CARTESIAN_POINT('Origin',(0.,13.25,0.));
#8750=CARTESIAN_POINT('',(-3.94762635814864E-16,11.7500000000001,-3.22348154659542));
#8751=CARTESIAN_POINT('Origin',(-2.5740463218088E-16,12.5,-2.10186832938358));
#8752=CARTESIAN_POINT('Origin',(0.,11.7500000000001,0.));
#8753=CARTESIAN_POINT('Origin',(0.,12.5,-9.15066633577766E-14));
#8754=CARTESIAN_POINT('',(-2.86797988869795,12.5,-9.18578895968479E-14));
#8755=CARTESIAN_POINT('',(2.86797988869795,12.5,-9.15066633577766E-14));
#8756=CARTESIAN_POINT('Origin',(0.,12.5,-9.15066633577766E-14));
#8757=CARTESIAN_POINT('',(0.,11.7500000000001,2.7681778559145));
#8758=CARTESIAN_POINT('Origin',(0.,11.7500000000001,0.));
#8759=CARTESIAN_POINT('',(0.,13.25,2.7681778559145));
#8760=CARTESIAN_POINT('Origin',(0.,13.25,0.));
#8761=CARTESIAN_POINT('Origin',(0.,13.25,2.7681778559145));
#8762=CARTESIAN_POINT('Origin',(0.,11.7500000000001,3.22348154659542));
#8763=CARTESIAN_POINT('Origin',(8.83883476483188,8.83883476483185,-6.72545142959742E-16));
#8764=CARTESIAN_POINT('',(9.36916485072177,9.36916485072174,-3.22348154659542));
#8765=CARTESIAN_POINT('Origin',(9.36916485072177,9.36916485072174,-7.12897851537325E-16));
#8766=CARTESIAN_POINT('',(8.30850467894199,8.30850467894196,-3.22348154659542));
#8767=CARTESIAN_POINT('Origin',(8.83883476483188,8.83883476483185,-2.10186832938358));
#8768=CARTESIAN_POINT('Origin',(8.30850467894199,8.30850467894196,-6.32192434382159E-16));
#8769=CARTESIAN_POINT('Origin',(8.83883476483188,8.83883476483185,-9.21792085007363E-14));
#8770=CARTESIAN_POINT('',(6.81086673722692,10.8668027924368,-9.2354821620272E-14));
#8771=CARTESIAN_POINT('',(10.8668027924368,6.81086673722688,-9.2354821620272E-14));
#8772=CARTESIAN_POINT('Origin',(8.83883476483188,8.83883476483185,-9.21792085007363E-14));
#8773=CARTESIAN_POINT('',(8.30850467894199,8.30850467894196,2.7681778559145));
#8774=CARTESIAN_POINT('Origin',(8.30850467894199,8.30850467894196,-6.32192434382159E-16));
#8775=CARTESIAN_POINT('',(9.36916485072177,9.36916485072174,2.7681778559145));
#8776=CARTESIAN_POINT('Origin',(9.36916485072177,9.36916485072174,-7.12897851537325E-16));
#8777=CARTESIAN_POINT('Origin',(9.36916485072177,9.36916485072174,2.7681778559145));
#8778=CARTESIAN_POINT('Origin',(8.30850467894199,8.30850467894196,3.22348154659542));
#8779=CARTESIAN_POINT('Origin',(12.5,-4.36435167355393E-14,-2.2962127484013E-15));
#8780=CARTESIAN_POINT('',(13.25,-4.52752211501344E-14,-3.22348154659542));
#8781=CARTESIAN_POINT('Origin',(13.25,-4.62621277396715E-14,-2.43398551330537E-15));
#8782=CARTESIAN_POINT('',(11.7500000000001,-4.00379991418698E-14,-3.22348154659542));
#8783=CARTESIAN_POINT('Origin',(12.5,-4.30000051550871E-14,-2.10186832938358));
#8784=CARTESIAN_POINT('Origin',(11.7500000000001,-4.1024905731407E-14,-2.15843998349723E-15));
#8785=CARTESIAN_POINT('Origin',(12.5,-4.36435167355393E-14,-9.38028761061779E-14));
#8786=CARTESIAN_POINT('',(12.5,2.86797988869791,-9.36272629866423E-14));
#8787=CARTESIAN_POINT('',(12.5,-2.86797988869799,-9.43297154647848E-14));
#8788=CARTESIAN_POINT('Origin',(12.5,-4.36435167355393E-14,-9.38028761061779E-14));
#8789=CARTESIAN_POINT('',(11.7500000000001,-4.15334117540145E-14,2.7681778559145));
#8790=CARTESIAN_POINT('Origin',(11.7500000000001,-4.1024905731407E-14,-2.15843998349723E-15));
#8791=CARTESIAN_POINT('',(13.25,-4.6770633762279E-14,2.7681778559145));
#8792=CARTESIAN_POINT('Origin',(13.25,-4.62621277396715E-14,-2.43398551330537E-15));
#8793=CARTESIAN_POINT('Origin',(13.25,-4.6770633762279E-14,2.7681778559145));
#8794=CARTESIAN_POINT('Origin',(11.7500000000001,-4.16170496851293E-14,
3.22348154659542));
#8795=CARTESIAN_POINT('Origin',(8.83883476483182,-8.83883476483191,-3.91988035384286E-15));
#8796=CARTESIAN_POINT('',(9.36916485072171,-9.3691648507218,-3.22348154659542));
#8797=CARTESIAN_POINT('Origin',(9.36916485072171,-9.36916485072181,-4.15507317507342E-15));
#8798=CARTESIAN_POINT('',(8.30850467894193,-8.30850467894202,-3.22348154659542));
#8799=CARTESIAN_POINT('Origin',(8.83883476483182,-8.83883476483191,-2.10186832938358));
#8800=CARTESIAN_POINT('Origin',(8.30850467894193,-8.30850467894202,-3.68468753261229E-15));
#8801=CARTESIAN_POINT('Origin',(8.83883476483182,-8.83883476483191,-9.54265437116194E-14));
#8802=CARTESIAN_POINT('',(10.8668027924368,-6.81086673722696,-9.48171106018132E-14));
#8803=CARTESIAN_POINT('',(6.81086673722685,-10.8668027924369,-9.63872030604969E-14));
#8804=CARTESIAN_POINT('Origin',(8.83883476483182,-8.83883476483191,-9.54265437116194E-14));
#8805=CARTESIAN_POINT('',(8.30850467894193,-8.30850467894202,2.7681778559145));
#8806=CARTESIAN_POINT('Origin',(8.30850467894193,-8.30850467894202,-3.68468753261229E-15));
#8807=CARTESIAN_POINT('',(9.36916485072171,-9.36916485072181,2.7681778559145));
#8808=CARTESIAN_POINT('Origin',(9.36916485072171,-9.36916485072181,-4.15507317507342E-15));
#8809=CARTESIAN_POINT('Origin',(9.36916485072171,-9.36916485072181,2.7681778559145));
#8810=CARTESIAN_POINT('Origin',(8.30850467894193,-8.30850467894202,3.22348154659542));
#8811=CARTESIAN_POINT('Origin',(0.,-12.5,-4.59242549680259E-15));
#8812=CARTESIAN_POINT('',(3.94762635814864E-16,-13.25,-3.22348154659542));
#8813=CARTESIAN_POINT('Origin',(0.,-13.25,-4.86797102661073E-15));
#8814=CARTESIAN_POINT('',(3.94762635814864E-16,-11.7500000000001,-3.22348154659542));
#8815=CARTESIAN_POINT('Origin',(2.5740463218088E-16,-12.5,-2.10186832938358));
#8816=CARTESIAN_POINT('Origin',(0.,-11.7500000000001,-4.31687996699444E-15));
#8817=CARTESIAN_POINT('Origin',(0.,-12.5,-9.60990888545792E-14));
#8818=CARTESIAN_POINT('',(2.86797988869795,-12.5,-9.64503150936505E-14));
#8819=CARTESIAN_POINT('',(-2.86797988869795,-12.5,-9.60990888545792E-14));
#8820=CARTESIAN_POINT('Origin',(0.,-12.5,-9.60990888545792E-14));
#8821=CARTESIAN_POINT('',(0.,-11.7500000000001,2.7681778559145));
#8822=CARTESIAN_POINT('Origin',(0.,-11.7500000000001,-4.31687996699444E-15));
#8823=CARTESIAN_POINT('',(0.,-13.25,2.7681778559145));
#8824=CARTESIAN_POINT('Origin',(0.,-13.25,-4.86797102661073E-15));
#8825=CARTESIAN_POINT('Origin',(0.,-13.25,2.7681778559145));
#8826=CARTESIAN_POINT('Origin',(0.,-11.7500000000001,3.22348154659542));
#8827=CARTESIAN_POINT('Origin',(-8.83883476483194,-8.83883476483179,-3.91988035384283E-15));
#8828=CARTESIAN_POINT('',(-9.36916485072184,-9.36916485072167,-3.22348154659542));
#8829=CARTESIAN_POINT('Origin',(-9.36916485072184,-9.36916485072167,-4.15507317507339E-15));
#8830=CARTESIAN_POINT('',(-8.30850467894205,-8.3085046789419,-3.22348154659542));
#8831=CARTESIAN_POINT('Origin',(-8.83883476483194,-8.83883476483179,-2.10186832938358));
#8832=CARTESIAN_POINT('Origin',(-8.30850467894205,-8.3085046789419,-3.68468753261227E-15));
#8833=CARTESIAN_POINT('Origin',(-8.83883476483194,-8.83883476483179,-9.54265437116194E-14));
#8834=CARTESIAN_POINT('',(-6.810866737227,-10.8668027924368,-9.63872030604969E-14));
#8835=CARTESIAN_POINT('',(-10.8668027924369,-6.81086673722681,-9.48171106018132E-14));
#8836=CARTESIAN_POINT('Origin',(-8.83883476483194,-8.83883476483179,-9.54265437116194E-14));
#8837=CARTESIAN_POINT('',(-8.30850467894205,-8.3085046789419,2.7681778559145));
#8838=CARTESIAN_POINT('Origin',(-8.30850467894205,-8.3085046789419,-3.68468753261227E-15));
#8839=CARTESIAN_POINT('',(-9.36916485072184,-9.36916485072168,2.7681778559145));
#8840=CARTESIAN_POINT('Origin',(-9.36916485072184,-9.36916485072167,-4.15507317507339E-15));
#8841=CARTESIAN_POINT('Origin',(-9.36916485072184,-9.36916485072168,2.7681778559145));
#8842=CARTESIAN_POINT('Origin',(-8.30850467894205,-8.3085046789419,3.22348154659542));
#8843=CARTESIAN_POINT('Origin',(-12.5,1.30930550206618E-13,-2.29621274840127E-15));
#8844=CARTESIAN_POINT('',(-13.25,1.38983764536922E-13,-3.22348154659542));
#8845=CARTESIAN_POINT('Origin',(-13.25,1.38786383219015E-13,-2.43398551330534E-15));
#8846=CARTESIAN_POINT('',(-11.7500000000001,1.23272098512128E-13,-3.22348154659542));
#8847=CARTESIAN_POINT('Origin',(-12.5,1.31059252522708E-13,-2.10186832938358));
#8848=CARTESIAN_POINT('Origin',(-11.7500000000001,1.23074717194221E-13,
-2.1584399834972E-15));
#8849=CARTESIAN_POINT('Origin',(-12.5,1.30930550206618E-13,-9.38028761061778E-14));
#8850=CARTESIAN_POINT('',(-12.5,-2.86797988869782,-9.46809417038561E-14));
#8851=CARTESIAN_POINT('',(-12.5,2.86797988869808,-9.32760367475709E-14));
#8852=CARTESIAN_POINT('Origin',(-12.5,1.30930550206618E-13,-9.38028761061778E-14));
#8853=CARTESIAN_POINT('',(-11.7500000000001,1.22566211171614E-13,2.7681778559145));
#8854=CARTESIAN_POINT('Origin',(-11.7500000000001,1.23074717194221E-13,
-2.1584399834972E-15));
#8855=CARTESIAN_POINT('',(-13.25,1.38277877196407E-13,2.7681778559145));
#8856=CARTESIAN_POINT('Origin',(-13.25,1.38786383219015E-13,-2.43398551330534E-15));
#8857=CARTESIAN_POINT('Origin',(-13.25,1.38277877196407E-13,2.7681778559145));
#8858=CARTESIAN_POINT('Origin',(-11.7500000000001,1.22482573240499E-13,
3.22348154659542));
#8859=CARTESIAN_POINT('Origin',(-8.83883476483176,8.83883476483197,-6.72545142959719E-16));
#8860=CARTESIAN_POINT('',(-9.36916485072164,9.36916485072187,-3.22348154659542));
#8861=CARTESIAN_POINT('Origin',(-9.36916485072164,9.36916485072187,-7.12897851537301E-16));
#8862=CARTESIAN_POINT('',(-8.30850467894187,8.30850467894208,-3.22348154659542));
#8863=CARTESIAN_POINT('Origin',(-8.83883476483176,8.83883476483197,-2.10186832938358));
#8864=CARTESIAN_POINT('Origin',(-8.30850467894187,8.30850467894208,-6.32192434382138E-16));
#8865=CARTESIAN_POINT('Origin',(-8.83883476483176,8.83883476483197,-9.21792085007363E-14));
#8866=CARTESIAN_POINT('',(-10.8668027924367,6.81086673722703,-9.2354821620272E-14));
#8867=CARTESIAN_POINT('',(-6.81086673722677,10.8668027924369,-9.2354821620272E-14));
#8868=CARTESIAN_POINT('Origin',(-8.83883476483176,8.83883476483197,-9.21792085007363E-14));
#8869=CARTESIAN_POINT('',(-8.30850467894187,8.30850467894208,2.7681778559145));
#8870=CARTESIAN_POINT('Origin',(-8.30850467894187,8.30850467894208,-6.32192434382138E-16));
#8871=CARTESIAN_POINT('',(-9.36916485072164,9.36916485072187,2.7681778559145));
#8872=CARTESIAN_POINT('Origin',(-9.36916485072164,9.36916485072187,-7.12897851537301E-16));
#8873=CARTESIAN_POINT('Origin',(-9.36916485072164,9.36916485072187,2.7681778559145));
#8874=CARTESIAN_POINT('Origin',(-8.30850467894187,8.30850467894208,3.22348154659542));
#8875=CARTESIAN_POINT('Origin',(0.,0.,0.916666666666667));
#8876=CARTESIAN_POINT('',(12.5,-1.53080849893419E-15,0.916666666666667));
#8877=CARTESIAN_POINT('Origin',(0.,0.,0.916666666666667));
#8878=CARTESIAN_POINT('',(12.5,-1.53080849893419E-15,-0.916666666666667));
#8879=CARTESIAN_POINT('',(12.5,-1.53080849893419E-15,0.916666666666667));
#8880=CARTESIAN_POINT('Origin',(0.,0.,-0.916666666666667));
#8881=CARTESIAN_POINT('Origin',(0.,0.,0.916666666666667));
#8882=CARTESIAN_POINT('',(13.25,-1.62265700887024E-15,-0.916666666666667));
#8883=CARTESIAN_POINT('Origin',(0.,0.,-0.916666666666667));
#8884=CARTESIAN_POINT('',(13.25,-1.62265700887024E-15,0.916666666666667));
#8885=CARTESIAN_POINT('',(13.25,-1.62265700887024E-15,0.916666666666667));
#8886=CARTESIAN_POINT('Origin',(0.,0.,0.916666666666667));
#8887=CARTESIAN_POINT('Origin',(0.,0.,0.916666666666667));
#8888=CARTESIAN_POINT('Origin',(0.,0.,-0.916666666666667));
#8889=CARTESIAN_POINT('Origin',(0.,1.12259289921848E-17,5.43888888888889));
#8890=CARTESIAN_POINT('',(-1.38214998470436E-15,-11.2861111111111,5.49999999999999));
#8891=CARTESIAN_POINT('Origin',(0.,7.71876610523947E-31,5.5));
#8892=CARTESIAN_POINT('',(-1.3746660320429E-15,-11.225,5.43888888888889));
#8893=CARTESIAN_POINT('Origin',(-1.38214998470436E-15,-11.2861111111111,
5.43888888888889));
#8894=CARTESIAN_POINT('',(1.3746660320429E-15,11.225,5.43888888888889));
#8895=CARTESIAN_POINT('Origin',(0.,1.12259289921847E-17,5.43888888888889));
#8896=CARTESIAN_POINT('Origin',(0.,1.12259289921847E-17,5.43888888888889));
#8897=CARTESIAN_POINT('Origin',(0.,1.12259289921848E-17,5.43888888888889));
#8898=CARTESIAN_POINT('',(1.68695096582548E-15,13.775,5.43888888888889));
#8899=CARTESIAN_POINT('',(-1.68695096582548E-15,-13.775,5.43888888888889));
#8900=CARTESIAN_POINT('Origin',(0.,1.12259289921848E-17,5.43888888888889));
#8901=CARTESIAN_POINT('Origin',(0.,1.12259289921848E-17,5.43888888888889));
#8902=CARTESIAN_POINT('',(-1.67946701316402E-15,-13.7138888888889,5.49999999999999));
#8903=CARTESIAN_POINT('Origin',(-1.67946701316402E-15,-13.7138888888889,
5.43888888888889));
#8904=CARTESIAN_POINT('Origin',(0.,7.71876610523947E-31,5.5));
#8905=CARTESIAN_POINT('Origin',(0.,0.,5.5));
#8906=CARTESIAN_POINT('',(-1.68695096582548E-15,13.775,5.09259259259259));
#8907=CARTESIAN_POINT('',(-1.68695096582548E-15,13.775,5.5));
#8908=CARTESIAN_POINT('',(1.70072824231589E-15,-13.775,5.09259259259259));
#8909=CARTESIAN_POINT('Origin',(0.,7.48395266145613E-17,5.09259259259259));
#8910=CARTESIAN_POINT('Origin',(0.,7.48395266145613E-17,5.09259259259259));
#8911=CARTESIAN_POINT('Origin',(0.,1.12259289921841E-16,4.88888888888888));
#8912=CARTESIAN_POINT('',(-1.7145055188063E-15,-14.,4.88888888888888));
#8913=CARTESIAN_POINT('Origin',(0.,1.12259289921841E-16,4.88888888888888));
#8914=CARTESIAN_POINT('',(-1.71450551880629E-15,-14.,4.88888888888888));
#8915=CARTESIAN_POINT('Origin',(0.,7.4839526614561E-17,5.09259259259259));
#8916=CARTESIAN_POINT('',(-1.34711147906209E-15,11.,4.88888888888889));
#8917=CARTESIAN_POINT('Origin',(0.,1.12259289921842E-16,4.88888888888888));
#8918=CARTESIAN_POINT('',(-1.3746660320429E-15,11.225,5.09259259259259));
#8919=CARTESIAN_POINT('',(-1.3746660320429E-15,11.225,5.09259259259259));
#8920=CARTESIAN_POINT('Origin',(0.,7.4839526614561E-17,5.09259259259259));
#8921=CARTESIAN_POINT('Origin',(0.,0.,5.5));
#8922=CARTESIAN_POINT('',(-1.3746660320429E-15,11.225,5.5));
#8923=CARTESIAN_POINT('Origin',(0.,13.775,5.5));
#8924=CARTESIAN_POINT('Origin',(0.,14.,4.88888888888889));
#8925=CARTESIAN_POINT('Origin',(0.,2.00944128960095E-15,-5.43888888888889));
#8926=CARTESIAN_POINT('',(-1.68695096582548E-15,13.775,-5.43888888888889));
#8927=CARTESIAN_POINT('Origin',(0.,2.00944128960095E-15,-5.4388888888889));
#8928=CARTESIAN_POINT('',(-1.67946701316402E-15,13.7138888888889,-5.5));
#8929=CARTESIAN_POINT('Origin',(-1.67946701316402E-15,13.7138888888889,
-5.43888888888889));
#8930=CARTESIAN_POINT('Origin',(0.,2.02066721859313E-15,-5.50000000000001));
#8931=CARTESIAN_POINT('Origin',(0.,2.00944128960095E-15,-5.43888888888889));
#8932=CARTESIAN_POINT('',(-1.38214998470436E-15,11.2861111111111,-5.5));
#8933=CARTESIAN_POINT('Origin',(0.,2.02066721859313E-15,-5.50000000000001));
#8934=CARTESIAN_POINT('',(-1.3746660320429E-15,11.225,-5.43888888888889));
#8935=CARTESIAN_POINT('Origin',(-1.38214998470436E-15,11.2861111111111,
-5.43888888888889));
#8936=CARTESIAN_POINT('Origin',(0.,2.00944128960095E-15,-5.43888888888889));
#8937=CARTESIAN_POINT('Origin',(0.,0.,5.5));
#8938=CARTESIAN_POINT('',(-1.3746660320429E-15,11.225,-5.0925925925926));
#8939=CARTESIAN_POINT('',(-1.3746660320429E-15,11.225,5.5));
#8940=CARTESIAN_POINT('',(1.3746660320429E-15,-11.225,-5.0925925925926));
#8941=CARTESIAN_POINT('Origin',(0.,1.94582769197857E-15,-5.0925925925926));
#8942=CARTESIAN_POINT('Origin',(0.,1.94582769197857E-15,-5.0925925925926));
#8943=CARTESIAN_POINT('Origin',(0.,1.90840792867129E-15,-4.88888888888889));
#8944=CARTESIAN_POINT('',(-1.34711147906209E-15,-11.,-4.8888888888889));
#8945=CARTESIAN_POINT('Origin',(0.,1.90840792867129E-15,-4.88888888888889));
#8946=CARTESIAN_POINT('',(-1.34711147906209E-15,-11.,-4.88888888888889));
#8947=CARTESIAN_POINT('Origin',(0.,1.94582769197857E-15,-5.0925925925926));
#8948=CARTESIAN_POINT('',(-1.7145055188063E-15,14.,-4.88888888888889));
#8949=CARTESIAN_POINT('Origin',(0.,1.90840792867129E-15,-4.88888888888889));
#8950=CARTESIAN_POINT('',(-1.68695096582548E-15,13.775,-5.09259259259259));
#8951=CARTESIAN_POINT('',(-1.68695096582548E-15,13.775,-5.0925925925926));
#8952=CARTESIAN_POINT('Origin',(0.,1.94582769197857E-15,-5.0925925925926));
#8953=CARTESIAN_POINT('Origin',(0.,0.,5.5));
#8954=CARTESIAN_POINT('',(-1.68695096582548E-15,13.775,5.5));
#8955=CARTESIAN_POINT('Origin',(0.,11.,-4.88888888888889));
#8956=CARTESIAN_POINT('Origin',(0.,13.775,-5.5));
#8957=CARTESIAN_POINT('',(0.,0.,0.));
#8958=CARTESIAN_POINT('Origin',(-28.795061332806,-41.6915321010441,20.));
#8959=CARTESIAN_POINT('',(-26.295061332806,-41.6915321010441,20.));
#8960=CARTESIAN_POINT('Origin',(-28.795061332806,-41.6915321010441,20.));
#8961=CARTESIAN_POINT('',(-26.295061332806,-41.6915321010441,1.76587979759228));
#8962=CARTESIAN_POINT('',(-26.295061332806,-41.6915321010441,20.));
#8963=CARTESIAN_POINT('',(-28.795061332806,-44.1915321010441,0.356833582029305));
#8964=CARTESIAN_POINT('Ctrl Pts',(-28.795061332806,-44.1915321010441,0.356833582029284));
#8965=CARTESIAN_POINT('Ctrl Pts',(-28.477785430142,-44.1915321010441,0.356833582029284));
#8966=CARTESIAN_POINT('Ctrl Pts',(-28.1469294547233,-44.1275251245074,0.406497032324426));
#8967=CARTESIAN_POINT('Ctrl Pts',(-27.5495967417843,-43.8830970093849,0.584048414544644));
#8968=CARTESIAN_POINT('Ctrl Pts',(-27.2824224552858,-43.7030327750914,0.710075190333896));
#8969=CARTESIAN_POINT('Ctrl Pts',(-26.8364104627744,-43.2788343380328,0.982143846508312));
#8970=CARTESIAN_POINT('Ctrl Pts',(-26.634884040132,-42.9955925725868,1.15080480840549));
#8971=CARTESIAN_POINT('Ctrl Pts',(-26.3640331527432,-42.3675807949546,1.47762784261656));
#8972=CARTESIAN_POINT('Ctrl Pts',(-26.295061332806,-42.0223600026362,1.63521545889971));
#8973=CARTESIAN_POINT('Ctrl Pts',(-26.295061332806,-41.6915321010441,1.76587979759228));
#8974=CARTESIAN_POINT('Ctrl Pts',(-26.295061332806,-41.6915321010441,1.76587979759228));
#8975=CARTESIAN_POINT('Ctrl Pts',(-26.295061332806,-41.3866319916517,1.88630365231953));
#8976=CARTESIAN_POINT('Ctrl Pts',(-26.3545217120232,-41.0538505476253,1.99948444500592));
#8977=CARTESIAN_POINT('Ctrl Pts',(-26.6094575005743,-40.432164168516,2.17871269254273));
#8978=CARTESIAN_POINT('Ctrl Pts',(-26.8052572776176,-40.14362590236,2.24556937536941));
#8979=CARTESIAN_POINT('Ctrl Pts',(-27.2559905957869,-39.697227181252,2.33582555282254));
#8980=CARTESIAN_POINT('Ctrl Pts',(-27.5353468960521,-39.5067960121042,2.36674372859812));
#8981=CARTESIAN_POINT('Ctrl Pts',(-28.1484345319317,-39.2539459288562,2.40438278535118));
#8982=CARTESIAN_POINT('Ctrl Pts',(-28.4821173645511,-39.1915321010441,2.41192340176922));
#8983=CARTESIAN_POINT('Ctrl Pts',(-29.1080053010609,-39.1915321010441,2.41192340176922));
#8984=CARTESIAN_POINT('Ctrl Pts',(-29.4416881336803,-39.2539459288562,2.40438278535118));
#8985=CARTESIAN_POINT('Ctrl Pts',(-30.0547757695599,-39.5067960121042,2.36674372859812));
#8986=CARTESIAN_POINT('Ctrl Pts',(-30.3341320698251,-39.697227181252,2.33582555282254));
#8987=CARTESIAN_POINT('Ctrl Pts',(-30.7848653879944,-40.14362590236,2.24556937536941));
#8988=CARTESIAN_POINT('Ctrl Pts',(-30.9806651650377,-40.432164168516,2.17871269254273));
#8989=CARTESIAN_POINT('Ctrl Pts',(-31.2356009535887,-41.0538505476253,1.99948444500592));
#8990=CARTESIAN_POINT('Ctrl Pts',(-31.295061332806,-41.3866319916517,1.88630365231953));
#8991=CARTESIAN_POINT('Ctrl Pts',(-31.295061332806,-42.0223600026362,1.63521545889971));
#8992=CARTESIAN_POINT('Ctrl Pts',(-31.2260895128688,-42.3675807949547,1.47762784261656));
#8993=CARTESIAN_POINT('Ctrl Pts',(-30.95523862548,-42.9955925725868,1.15080480840548));
#8994=CARTESIAN_POINT('Ctrl Pts',(-30.7537122028376,-43.2788343380328,0.982143846508312));
#8995=CARTESIAN_POINT('Ctrl Pts',(-30.3077002103262,-43.7030327750914,0.710075190333895));
#8996=CARTESIAN_POINT('Ctrl Pts',(-30.0405259238277,-43.8830970093849,0.584048414544644));
#8997=CARTESIAN_POINT('Ctrl Pts',(-29.4431932108887,-44.1275251245074,0.406497032324426));
#8998=CARTESIAN_POINT('Ctrl Pts',(-29.11233723547,-44.1915321010441,0.356833582029284));
#8999=CARTESIAN_POINT('Ctrl Pts',(-28.795061332806,-44.1915321010441,0.356833582029284));
#9000=CARTESIAN_POINT('Origin',(-28.795061332806,-41.6915321010441,20.));
#9001=CARTESIAN_POINT('',(-28.795061332806,-44.1915321010441,-16.3568335820293));
#9002=CARTESIAN_POINT('',(-26.295061332806,-41.6915321010441,-17.7658797975923));
#9003=CARTESIAN_POINT('Ctrl Pts',(-28.795061332806,-44.1915321010441,-16.3568335820293));
#9004=CARTESIAN_POINT('Ctrl Pts',(-29.1123372354701,-44.1915321010441,-16.3568335820293));
#9005=CARTESIAN_POINT('Ctrl Pts',(-29.4431932108887,-44.1275251245074,-16.4064970323244));
#9006=CARTESIAN_POINT('Ctrl Pts',(-30.0405259238277,-43.8830970093849,-16.5840484145446));
#9007=CARTESIAN_POINT('Ctrl Pts',(-30.3077002103262,-43.7030327750914,-16.7100751903339));
#9008=CARTESIAN_POINT('Ctrl Pts',(-30.7537122028376,-43.2788343380328,-16.9821438465083));
#9009=CARTESIAN_POINT('Ctrl Pts',(-30.95523862548,-42.9955925725868,-17.1508048084055));
#9010=CARTESIAN_POINT('Ctrl Pts',(-31.2260895128688,-42.3675807949546,-17.4776278426165));
#9011=CARTESIAN_POINT('Ctrl Pts',(-31.295061332806,-42.0223600026362,-17.6352154588997));
#9012=CARTESIAN_POINT('Ctrl Pts',(-31.295061332806,-41.3866319916517,-17.8863036523195));
#9013=CARTESIAN_POINT('Ctrl Pts',(-31.2356009535887,-41.0538505476253,-17.9994844450059));
#9014=CARTESIAN_POINT('Ctrl Pts',(-30.9806651650377,-40.432164168516,-18.1787126925427));
#9015=CARTESIAN_POINT('Ctrl Pts',(-30.7848653879944,-40.14362590236,-18.2455693753694));
#9016=CARTESIAN_POINT('Ctrl Pts',(-30.3341320698251,-39.697227181252,-18.3358255528225));
#9017=CARTESIAN_POINT('Ctrl Pts',(-30.0547757695599,-39.5067960121042,-18.3667437285981));
#9018=CARTESIAN_POINT('Ctrl Pts',(-29.4416881336803,-39.2539459288562,-18.4043827853512));
#9019=CARTESIAN_POINT('Ctrl Pts',(-29.1080053010609,-39.1915321010441,-18.4119234017692));
#9020=CARTESIAN_POINT('Ctrl Pts',(-28.4821173645511,-39.1915321010441,-18.4119234017692));
#9021=CARTESIAN_POINT('Ctrl Pts',(-28.1484345319317,-39.2539459288562,-18.4043827853512));
#9022=CARTESIAN_POINT('Ctrl Pts',(-27.5353468960521,-39.5067960121042,-18.3667437285981));
#9023=CARTESIAN_POINT('Ctrl Pts',(-27.2559905957869,-39.697227181252,-18.3358255528225));
#9024=CARTESIAN_POINT('Ctrl Pts',(-26.8052572776176,-40.14362590236,-18.2455693753694));
#9025=CARTESIAN_POINT('Ctrl Pts',(-26.6094575005743,-40.432164168516,-18.1787126925427));
#9026=CARTESIAN_POINT('Ctrl Pts',(-26.3545217120232,-41.0538505476253,-17.9994844450059));
#9027=CARTESIAN_POINT('Ctrl Pts',(-26.295061332806,-41.3866319916517,-17.8863036523195));
#9028=CARTESIAN_POINT('Ctrl Pts',(-26.295061332806,-41.6915321010441,-17.7658797975923));
#9029=CARTESIAN_POINT('Ctrl Pts',(-26.295061332806,-41.6915321010441,-17.7658797975923));
#9030=CARTESIAN_POINT('Ctrl Pts',(-26.295061332806,-42.0223600026362,-17.6352154588997));
#9031=CARTESIAN_POINT('Ctrl Pts',(-26.3640331527432,-42.3675807949547,-17.4776278426165));
#9032=CARTESIAN_POINT('Ctrl Pts',(-26.634884040132,-42.9955925725868,-17.1508048084055));
#9033=CARTESIAN_POINT('Ctrl Pts',(-26.8364104627744,-43.2788343380328,-16.9821438465083));
#9034=CARTESIAN_POINT('Ctrl Pts',(-27.2824224552858,-43.7030327750914,-16.7100751903339));
#9035=CARTESIAN_POINT('Ctrl Pts',(-27.5495967417843,-43.8830970093849,-16.5840484145446));
#9036=CARTESIAN_POINT('Ctrl Pts',(-28.1469294547233,-44.1275251245074,-16.4064970323244));
#9037=CARTESIAN_POINT('Ctrl Pts',(-28.477785430142,-44.1915321010441,-16.3568335820293));
#9038=CARTESIAN_POINT('Ctrl Pts',(-28.795061332806,-44.1915321010441,-16.3568335820293));
#9039=CARTESIAN_POINT('',(-26.295061332806,-41.6915321010441,-20.));
#9040=CARTESIAN_POINT('',(-26.295061332806,-41.6915321010441,20.));
#9041=CARTESIAN_POINT('Origin',(-28.795061332806,-41.6915321010441,-20.));
#9042=CARTESIAN_POINT('Origin',(28.795061332806,41.6915321010441,20.));
#9043=CARTESIAN_POINT('',(31.295061332806,41.6915321010441,20.));
#9044=CARTESIAN_POINT('Origin',(28.795061332806,41.6915321010441,20.));
#9045=CARTESIAN_POINT('',(31.295061332806,41.6915321010441,1.76587979759228));
#9046=CARTESIAN_POINT('',(31.295061332806,41.6915321010441,20.));
#9047=CARTESIAN_POINT('',(28.795061332806,44.1915321010441,0.356833582029305));
#9048=CARTESIAN_POINT('Ctrl Pts',(28.795061332806,44.1915321010441,0.356833582029284));
#9049=CARTESIAN_POINT('Ctrl Pts',(28.477785430142,44.1915321010441,0.356833582029284));
#9050=CARTESIAN_POINT('Ctrl Pts',(28.1469294547233,44.1275251245074,0.406497032324426));
#9051=CARTESIAN_POINT('Ctrl Pts',(27.5495967417843,43.8830970093849,0.584048414544644));
#9052=CARTESIAN_POINT('Ctrl Pts',(27.2824224552858,43.7030327750914,0.710075190333896));
#9053=CARTESIAN_POINT('Ctrl Pts',(26.8364104627744,43.2788343380328,0.982143846508312));
#9054=CARTESIAN_POINT('Ctrl Pts',(26.634884040132,42.9955925725868,1.15080480840549));
#9055=CARTESIAN_POINT('Ctrl Pts',(26.3640331527432,42.3675807949546,1.47762784261656));
#9056=CARTESIAN_POINT('Ctrl Pts',(26.295061332806,42.0223600026362,1.63521545889971));
#9057=CARTESIAN_POINT('Ctrl Pts',(26.295061332806,41.3866319916517,1.88630365231953));
#9058=CARTESIAN_POINT('Ctrl Pts',(26.3545217120232,41.0538505476253,1.99948444500592));
#9059=CARTESIAN_POINT('Ctrl Pts',(26.6094575005743,40.432164168516,2.17871269254273));
#9060=CARTESIAN_POINT('Ctrl Pts',(26.8052572776176,40.14362590236,2.24556937536941));
#9061=CARTESIAN_POINT('Ctrl Pts',(27.2559905957869,39.697227181252,2.33582555282254));
#9062=CARTESIAN_POINT('Ctrl Pts',(27.5353468960521,39.5067960121042,2.36674372859812));
#9063=CARTESIAN_POINT('Ctrl Pts',(28.1484345319317,39.2539459288562,2.40438278535118));
#9064=CARTESIAN_POINT('Ctrl Pts',(28.4821173645511,39.1915321010441,2.41192340176922));
#9065=CARTESIAN_POINT('Ctrl Pts',(29.1080053010609,39.1915321010441,2.41192340176922));
#9066=CARTESIAN_POINT('Ctrl Pts',(29.4416881336803,39.2539459288562,2.40438278535118));
#9067=CARTESIAN_POINT('Ctrl Pts',(30.0547757695599,39.5067960121042,2.36674372859812));
#9068=CARTESIAN_POINT('Ctrl Pts',(30.3341320698251,39.697227181252,2.33582555282254));
#9069=CARTESIAN_POINT('Ctrl Pts',(30.7848653879944,40.14362590236,2.24556937536941));
#9070=CARTESIAN_POINT('Ctrl Pts',(30.9806651650377,40.432164168516,2.17871269254273));
#9071=CARTESIAN_POINT('Ctrl Pts',(31.2356009535887,41.0538505476253,1.99948444500592));
#9072=CARTESIAN_POINT('Ctrl Pts',(31.295061332806,41.3866319916517,1.88630365231953));
#9073=CARTESIAN_POINT('Ctrl Pts',(31.295061332806,41.6915321010441,1.76587979759227));
#9074=CARTESIAN_POINT('Ctrl Pts',(31.295061332806,41.6915321010441,1.76587979759227));
#9075=CARTESIAN_POINT('Ctrl Pts',(31.295061332806,42.0223600026362,1.63521545889971));
#9076=CARTESIAN_POINT('Ctrl Pts',(31.2260895128688,42.3675807949547,1.47762784261656));
#9077=CARTESIAN_POINT('Ctrl Pts',(30.95523862548,42.9955925725868,1.15080480840548));
#9078=CARTESIAN_POINT('Ctrl Pts',(30.7537122028376,43.2788343380328,0.982143846508312));
#9079=CARTESIAN_POINT('Ctrl Pts',(30.3077002103262,43.7030327750914,0.710075190333895));
#9080=CARTESIAN_POINT('Ctrl Pts',(30.0405259238277,43.8830970093849,0.584048414544644));
#9081=CARTESIAN_POINT('Ctrl Pts',(29.4431932108887,44.1275251245074,0.406497032324426));
#9082=CARTESIAN_POINT('Ctrl Pts',(29.11233723547,44.1915321010441,0.356833582029284));
#9083=CARTESIAN_POINT('Ctrl Pts',(28.795061332806,44.1915321010441,0.356833582029284));
#9084=CARTESIAN_POINT('Origin',(28.795061332806,41.6915321010441,20.));
#9085=CARTESIAN_POINT('',(28.795061332806,44.1915321010441,-16.3568335820293));
#9086=CARTESIAN_POINT('',(31.295061332806,41.6915321010441,-17.7658797975923));
#9087=CARTESIAN_POINT('Ctrl Pts',(28.795061332806,44.1915321010441,-16.3568335820293));
#9088=CARTESIAN_POINT('Ctrl Pts',(29.1123372354701,44.1915321010441,-16.3568335820293));
#9089=CARTESIAN_POINT('Ctrl Pts',(29.4431932108887,44.1275251245074,-16.4064970323244));
#9090=CARTESIAN_POINT('Ctrl Pts',(30.0405259238277,43.8830970093849,-16.5840484145446));
#9091=CARTESIAN_POINT('Ctrl Pts',(30.3077002103262,43.7030327750914,-16.7100751903339));
#9092=CARTESIAN_POINT('Ctrl Pts',(30.7537122028376,43.2788343380328,-16.9821438465083));
#9093=CARTESIAN_POINT('Ctrl Pts',(30.95523862548,42.9955925725868,-17.1508048084055));
#9094=CARTESIAN_POINT('Ctrl Pts',(31.2260895128688,42.3675807949546,-17.4776278426165));
#9095=CARTESIAN_POINT('Ctrl Pts',(31.295061332806,42.0223600026362,-17.6352154588997));
#9096=CARTESIAN_POINT('Ctrl Pts',(31.295061332806,41.6915321010441,-17.7658797975923));
#9097=CARTESIAN_POINT('Ctrl Pts',(31.295061332806,41.6915321010441,-17.7658797975923));
#9098=CARTESIAN_POINT('Ctrl Pts',(31.295061332806,41.3866319916517,-17.8863036523195));
#9099=CARTESIAN_POINT('Ctrl Pts',(31.2356009535887,41.0538505476253,-17.9994844450059));
#9100=CARTESIAN_POINT('Ctrl Pts',(30.9806651650377,40.432164168516,-18.1787126925427));
#9101=CARTESIAN_POINT('Ctrl Pts',(30.7848653879944,40.14362590236,-18.2455693753694));
#9102=CARTESIAN_POINT('Ctrl Pts',(30.3341320698251,39.697227181252,-18.3358255528225));
#9103=CARTESIAN_POINT('Ctrl Pts',(30.0547757695599,39.5067960121042,-18.3667437285981));
#9104=CARTESIAN_POINT('Ctrl Pts',(29.4416881336803,39.2539459288562,-18.4043827853512));
#9105=CARTESIAN_POINT('Ctrl Pts',(29.1080053010609,39.1915321010441,-18.4119234017692));
#9106=CARTESIAN_POINT('Ctrl Pts',(28.4821173645511,39.1915321010441,-18.4119234017692));
#9107=CARTESIAN_POINT('Ctrl Pts',(28.1484345319317,39.2539459288562,-18.4043827853512));
#9108=CARTESIAN_POINT('Ctrl Pts',(27.5353468960521,39.5067960121042,-18.3667437285981));
#9109=CARTESIAN_POINT('Ctrl Pts',(27.2559905957869,39.697227181252,-18.3358255528225));
#9110=CARTESIAN_POINT('Ctrl Pts',(26.8052572776176,40.14362590236,-18.2455693753694));
#9111=CARTESIAN_POINT('Ctrl Pts',(26.6094575005743,40.432164168516,-18.1787126925427));
#9112=CARTESIAN_POINT('Ctrl Pts',(26.3545217120232,41.0538505476253,-17.9994844450059));
#9113=CARTESIAN_POINT('Ctrl Pts',(26.295061332806,41.3866319916517,-17.8863036523195));
#9114=CARTESIAN_POINT('Ctrl Pts',(26.295061332806,42.0223600026362,-17.6352154588997));
#9115=CARTESIAN_POINT('Ctrl Pts',(26.3640331527432,42.3675807949547,-17.4776278426165));
#9116=CARTESIAN_POINT('Ctrl Pts',(26.634884040132,42.9955925725868,-17.1508048084055));
#9117=CARTESIAN_POINT('Ctrl Pts',(26.8364104627744,43.2788343380328,-16.9821438465083));
#9118=CARTESIAN_POINT('Ctrl Pts',(27.2824224552858,43.7030327750914,-16.7100751903339));
#9119=CARTESIAN_POINT('Ctrl Pts',(27.5495967417843,43.8830970093849,-16.5840484145446));
#9120=CARTESIAN_POINT('Ctrl Pts',(28.1469294547233,44.1275251245074,-16.4064970323244));
#9121=CARTESIAN_POINT('Ctrl Pts',(28.477785430142,44.1915321010441,-16.3568335820293));
#9122=CARTESIAN_POINT('Ctrl Pts',(28.795061332806,44.1915321010441,-16.3568335820293));
#9123=CARTESIAN_POINT('',(31.295061332806,41.6915321010441,-20.));
#9124=CARTESIAN_POINT('',(31.295061332806,41.6915321010441,20.));
#9125=CARTESIAN_POINT('Origin',(28.795061332806,41.6915321010441,-20.));
#9126=CARTESIAN_POINT('Origin',(28.795061332806,-41.6915321010441,20.));
#9127=CARTESIAN_POINT('',(31.295061332806,-41.6915321010441,20.));
#9128=CARTESIAN_POINT('Origin',(28.795061332806,-41.6915321010441,20.));
#9129=CARTESIAN_POINT('',(31.295061332806,-41.6915321010441,1.76587979759228));
#9130=CARTESIAN_POINT('',(31.295061332806,-41.6915321010441,20.));
#9131=CARTESIAN_POINT('',(28.795061332806,-44.1915321010441,0.356833582029306));
#9132=CARTESIAN_POINT('Ctrl Pts',(28.795061332806,-44.1915321010441,0.356833582029284));
#9133=CARTESIAN_POINT('Ctrl Pts',(29.1123372354701,-44.1915321010441,0.356833582029283));
#9134=CARTESIAN_POINT('Ctrl Pts',(29.4431932108887,-44.1275251245074,0.406497032324425));
#9135=CARTESIAN_POINT('Ctrl Pts',(30.0405259238277,-43.8830970093849,0.584048414544644));
#9136=CARTESIAN_POINT('Ctrl Pts',(30.3077002103262,-43.7030327750914,0.710075190333896));
#9137=CARTESIAN_POINT('Ctrl Pts',(30.7537122028376,-43.2788343380328,0.982143846508312));
#9138=CARTESIAN_POINT('Ctrl Pts',(30.95523862548,-42.9955925725868,1.15080480840548));
#9139=CARTESIAN_POINT('Ctrl Pts',(31.2260895128688,-42.3675807949546,1.47762784261656));
#9140=CARTESIAN_POINT('Ctrl Pts',(31.295061332806,-42.0223600026362,1.63521545889971));
#9141=CARTESIAN_POINT('Ctrl Pts',(31.295061332806,-41.6915321010441,1.76587979759228));
#9142=CARTESIAN_POINT('Ctrl Pts',(31.295061332806,-41.6915321010441,1.76587979759228));
#9143=CARTESIAN_POINT('Ctrl Pts',(31.295061332806,-41.3866319916517,1.88630365231953));
#9144=CARTESIAN_POINT('Ctrl Pts',(31.2356009535887,-41.0538505476253,1.99948444500592));
#9145=CARTESIAN_POINT('Ctrl Pts',(30.9806651650377,-40.432164168516,2.17871269254273));
#9146=CARTESIAN_POINT('Ctrl Pts',(30.7848653879944,-40.14362590236,2.24556937536941));
#9147=CARTESIAN_POINT('Ctrl Pts',(30.3341320698251,-39.697227181252,2.33582555282254));
#9148=CARTESIAN_POINT('Ctrl Pts',(30.0547757695599,-39.5067960121042,2.36674372859812));
#9149=CARTESIAN_POINT('Ctrl Pts',(29.4416881336803,-39.2539459288562,2.40438278535118));
#9150=CARTESIAN_POINT('Ctrl Pts',(29.1080053010609,-39.1915321010441,2.41192340176922));
#9151=CARTESIAN_POINT('Ctrl Pts',(28.4821173645511,-39.1915321010441,2.41192340176922));
#9152=CARTESIAN_POINT('Ctrl Pts',(28.1484345319317,-39.2539459288562,2.40438278535118));
#9153=CARTESIAN_POINT('Ctrl Pts',(27.5353468960521,-39.5067960121042,2.36674372859812));
#9154=CARTESIAN_POINT('Ctrl Pts',(27.2559905957869,-39.697227181252,2.33582555282254));
#9155=CARTESIAN_POINT('Ctrl Pts',(26.8052572776176,-40.14362590236,2.24556937536941));
#9156=CARTESIAN_POINT('Ctrl Pts',(26.6094575005743,-40.432164168516,2.17871269254273));
#9157=CARTESIAN_POINT('Ctrl Pts',(26.3545217120232,-41.0538505476253,1.99948444500592));
#9158=CARTESIAN_POINT('Ctrl Pts',(26.295061332806,-41.3866319916517,1.88630365231953));
#9159=CARTESIAN_POINT('Ctrl Pts',(26.295061332806,-42.0223600026362,1.63521545889971));
#9160=CARTESIAN_POINT('Ctrl Pts',(26.3640331527432,-42.3675807949547,1.47762784261656));
#9161=CARTESIAN_POINT('Ctrl Pts',(26.634884040132,-42.9955925725868,1.15080480840548));
#9162=CARTESIAN_POINT('Ctrl Pts',(26.8364104627744,-43.2788343380328,0.982143846508312));
#9163=CARTESIAN_POINT('Ctrl Pts',(27.2824224552858,-43.7030327750914,0.710075190333895));
#9164=CARTESIAN_POINT('Ctrl Pts',(27.5495967417843,-43.8830970093849,0.584048414544644));
#9165=CARTESIAN_POINT('Ctrl Pts',(28.1469294547233,-44.1275251245074,0.406497032324426));
#9166=CARTESIAN_POINT('Ctrl Pts',(28.4777854301419,-44.1915321010441,0.356833582029285));
#9167=CARTESIAN_POINT('Ctrl Pts',(28.795061332806,-44.1915321010441,0.356833582029285));
#9168=CARTESIAN_POINT('Origin',(28.795061332806,-41.6915321010441,20.));
#9169=CARTESIAN_POINT('',(28.795061332806,-44.1915321010441,-16.3568335820293));
#9170=CARTESIAN_POINT('',(31.295061332806,-41.6915321010441,-17.7658797975923));
#9171=CARTESIAN_POINT('Ctrl Pts',(28.795061332806,-44.1915321010441,-16.3568335820293));
#9172=CARTESIAN_POINT('Ctrl Pts',(28.4777854301419,-44.1915321010441,-16.3568335820293));
#9173=CARTESIAN_POINT('Ctrl Pts',(28.1469294547233,-44.1275251245074,-16.4064970323244));
#9174=CARTESIAN_POINT('Ctrl Pts',(27.5495967417843,-43.8830970093849,-16.5840484145446));
#9175=CARTESIAN_POINT('Ctrl Pts',(27.2824224552858,-43.7030327750914,-16.7100751903339));
#9176=CARTESIAN_POINT('Ctrl Pts',(26.8364104627744,-43.2788343380328,-16.9821438465083));
#9177=CARTESIAN_POINT('Ctrl Pts',(26.634884040132,-42.9955925725868,-17.1508048084055));
#9178=CARTESIAN_POINT('Ctrl Pts',(26.3640331527432,-42.3675807949546,-17.4776278426165));
#9179=CARTESIAN_POINT('Ctrl Pts',(26.295061332806,-42.0223600026362,-17.6352154588997));
#9180=CARTESIAN_POINT('Ctrl Pts',(26.295061332806,-41.3866319916517,-17.8863036523195));
#9181=CARTESIAN_POINT('Ctrl Pts',(26.3545217120232,-41.0538505476253,-17.9994844450059));
#9182=CARTESIAN_POINT('Ctrl Pts',(26.6094575005743,-40.432164168516,-18.1787126925427));
#9183=CARTESIAN_POINT('Ctrl Pts',(26.8052572776176,-40.14362590236,-18.2455693753694));
#9184=CARTESIAN_POINT('Ctrl Pts',(27.2559905957869,-39.697227181252,-18.3358255528225));
#9185=CARTESIAN_POINT('Ctrl Pts',(27.5353468960521,-39.5067960121042,-18.3667437285981));
#9186=CARTESIAN_POINT('Ctrl Pts',(28.1484345319317,-39.2539459288562,-18.4043827853512));
#9187=CARTESIAN_POINT('Ctrl Pts',(28.4821173645511,-39.1915321010441,-18.4119234017692));
#9188=CARTESIAN_POINT('Ctrl Pts',(29.1080053010609,-39.1915321010441,-18.4119234017692));
#9189=CARTESIAN_POINT('Ctrl Pts',(29.4416881336803,-39.2539459288562,-18.4043827853512));
#9190=CARTESIAN_POINT('Ctrl Pts',(30.0547757695599,-39.5067960121042,-18.3667437285981));
#9191=CARTESIAN_POINT('Ctrl Pts',(30.3341320698251,-39.697227181252,-18.3358255528225));
#9192=CARTESIAN_POINT('Ctrl Pts',(30.7848653879944,-40.14362590236,-18.2455693753694));
#9193=CARTESIAN_POINT('Ctrl Pts',(30.9806651650377,-40.432164168516,-18.1787126925427));
#9194=CARTESIAN_POINT('Ctrl Pts',(31.2356009535887,-41.0538505476253,-17.9994844450059));
#9195=CARTESIAN_POINT('Ctrl Pts',(31.295061332806,-41.3866319916517,-17.8863036523195));
#9196=CARTESIAN_POINT('Ctrl Pts',(31.295061332806,-41.6915321010441,-17.7658797975923));
#9197=CARTESIAN_POINT('Ctrl Pts',(31.295061332806,-41.6915321010441,-17.7658797975923));
#9198=CARTESIAN_POINT('Ctrl Pts',(31.295061332806,-42.0223600026362,-17.6352154588997));
#9199=CARTESIAN_POINT('Ctrl Pts',(31.2260895128688,-42.3675807949546,-17.4776278426165));
#9200=CARTESIAN_POINT('Ctrl Pts',(30.95523862548,-42.9955925725868,-17.1508048084055));
#9201=CARTESIAN_POINT('Ctrl Pts',(30.7537122028376,-43.2788343380328,-16.9821438465083));
#9202=CARTESIAN_POINT('Ctrl Pts',(30.3077002103262,-43.7030327750914,-16.7100751903339));
#9203=CARTESIAN_POINT('Ctrl Pts',(30.0405259238277,-43.8830970093849,-16.5840484145446));
#9204=CARTESIAN_POINT('Ctrl Pts',(29.4431932108887,-44.1275251245074,-16.4064970323244));
#9205=CARTESIAN_POINT('Ctrl Pts',(29.11233723547,-44.1915321010441,-16.3568335820293));
#9206=CARTESIAN_POINT('Ctrl Pts',(28.795061332806,-44.1915321010441,-16.3568335820293));
#9207=CARTESIAN_POINT('',(31.295061332806,-41.6915321010441,-20.));
#9208=CARTESIAN_POINT('',(31.295061332806,-41.6915321010441,20.));
#9209=CARTESIAN_POINT('Origin',(28.795061332806,-41.6915321010441,-20.));
#9210=CARTESIAN_POINT('Origin',(-28.795061332806,41.6915321010441,20.));
#9211=CARTESIAN_POINT('',(-26.295061332806,41.6915321010441,20.));
#9212=CARTESIAN_POINT('Origin',(-28.795061332806,41.6915321010441,20.));
#9213=CARTESIAN_POINT('',(-26.295061332806,41.6915321010441,1.76587979759228));
#9214=CARTESIAN_POINT('',(-26.295061332806,41.6915321010441,20.));
#9215=CARTESIAN_POINT('',(-28.795061332806,44.1915321010441,0.356833582029306));
#9216=CARTESIAN_POINT('Ctrl Pts',(-28.795061332806,44.1915321010441,0.356833582029283));
#9217=CARTESIAN_POINT('Ctrl Pts',(-29.1123372354701,44.1915321010441,0.356833582029283));
#9218=CARTESIAN_POINT('Ctrl Pts',(-29.4431932108887,44.1275251245074,0.406497032324425));
#9219=CARTESIAN_POINT('Ctrl Pts',(-30.0405259238277,43.8830970093849,0.584048414544644));
#9220=CARTESIAN_POINT('Ctrl Pts',(-30.3077002103262,43.7030327750914,0.710075190333896));
#9221=CARTESIAN_POINT('Ctrl Pts',(-30.7537122028376,43.2788343380328,0.982143846508312));
#9222=CARTESIAN_POINT('Ctrl Pts',(-30.95523862548,42.9955925725868,1.15080480840548));
#9223=CARTESIAN_POINT('Ctrl Pts',(-31.2260895128688,42.3675807949546,1.47762784261656));
#9224=CARTESIAN_POINT('Ctrl Pts',(-31.295061332806,42.0223600026362,1.63521545889971));
#9225=CARTESIAN_POINT('Ctrl Pts',(-31.295061332806,41.3866319916517,1.88630365231953));
#9226=CARTESIAN_POINT('Ctrl Pts',(-31.2356009535887,41.0538505476253,1.99948444500592));
#9227=CARTESIAN_POINT('Ctrl Pts',(-30.9806651650377,40.432164168516,2.17871269254273));
#9228=CARTESIAN_POINT('Ctrl Pts',(-30.7848653879944,40.14362590236,2.24556937536941));
#9229=CARTESIAN_POINT('Ctrl Pts',(-30.3341320698251,39.697227181252,2.33582555282254));
#9230=CARTESIAN_POINT('Ctrl Pts',(-30.0547757695599,39.5067960121042,2.36674372859812));
#9231=CARTESIAN_POINT('Ctrl Pts',(-29.4416881336803,39.2539459288562,2.40438278535118));
#9232=CARTESIAN_POINT('Ctrl Pts',(-29.1080053010609,39.1915321010441,2.41192340176922));
#9233=CARTESIAN_POINT('Ctrl Pts',(-28.4821173645511,39.1915321010441,2.41192340176922));
#9234=CARTESIAN_POINT('Ctrl Pts',(-28.1484345319317,39.2539459288562,2.40438278535118));
#9235=CARTESIAN_POINT('Ctrl Pts',(-27.5353468960521,39.5067960121042,2.36674372859812));
#9236=CARTESIAN_POINT('Ctrl Pts',(-27.2559905957869,39.697227181252,2.33582555282254));
#9237=CARTESIAN_POINT('Ctrl Pts',(-26.8052572776176,40.14362590236,2.24556937536941));
#9238=CARTESIAN_POINT('Ctrl Pts',(-26.6094575005743,40.432164168516,2.17871269254273));
#9239=CARTESIAN_POINT('Ctrl Pts',(-26.3545217120232,41.0538505476253,1.99948444500592));
#9240=CARTESIAN_POINT('Ctrl Pts',(-26.295061332806,41.3866319916517,1.88630365231953));
#9241=CARTESIAN_POINT('Ctrl Pts',(-26.295061332806,41.6915321010441,1.76587979759227));
#9242=CARTESIAN_POINT('Ctrl Pts',(-26.295061332806,41.6915321010441,1.76587979759227));
#9243=CARTESIAN_POINT('Ctrl Pts',(-26.295061332806,42.0223600026362,1.63521545889971));
#9244=CARTESIAN_POINT('Ctrl Pts',(-26.3640331527432,42.3675807949547,1.47762784261656));
#9245=CARTESIAN_POINT('Ctrl Pts',(-26.634884040132,42.9955925725868,1.15080480840548));
#9246=CARTESIAN_POINT('Ctrl Pts',(-26.8364104627744,43.2788343380328,0.982143846508312));
#9247=CARTESIAN_POINT('Ctrl Pts',(-27.2824224552858,43.7030327750914,0.710075190333895));
#9248=CARTESIAN_POINT('Ctrl Pts',(-27.5495967417843,43.8830970093849,0.584048414544644));
#9249=CARTESIAN_POINT('Ctrl Pts',(-28.1469294547233,44.1275251245074,0.406497032324426));
#9250=CARTESIAN_POINT('Ctrl Pts',(-28.4777854301419,44.1915321010441,0.356833582029285));
#9251=CARTESIAN_POINT('Ctrl Pts',(-28.795061332806,44.1915321010441,0.356833582029285));
#9252=CARTESIAN_POINT('Origin',(-28.795061332806,41.6915321010441,20.));
#9253=CARTESIAN_POINT('',(-28.795061332806,44.1915321010441,-16.3568335820293));
#9254=CARTESIAN_POINT('',(-26.295061332806,41.6915321010441,-17.7658797975923));
#9255=CARTESIAN_POINT('Ctrl Pts',(-28.795061332806,44.1915321010441,-16.3568335820293));
#9256=CARTESIAN_POINT('Ctrl Pts',(-28.4777854301419,44.1915321010441,-16.3568335820293));
#9257=CARTESIAN_POINT('Ctrl Pts',(-28.1469294547233,44.1275251245074,-16.4064970323244));
#9258=CARTESIAN_POINT('Ctrl Pts',(-27.5495967417843,43.8830970093849,-16.5840484145446));
#9259=CARTESIAN_POINT('Ctrl Pts',(-27.2824224552858,43.7030327750914,-16.7100751903339));
#9260=CARTESIAN_POINT('Ctrl Pts',(-26.8364104627744,43.2788343380328,-16.9821438465083));
#9261=CARTESIAN_POINT('Ctrl Pts',(-26.634884040132,42.9955925725868,-17.1508048084055));
#9262=CARTESIAN_POINT('Ctrl Pts',(-26.3640331527432,42.3675807949546,-17.4776278426165));
#9263=CARTESIAN_POINT('Ctrl Pts',(-26.295061332806,42.0223600026362,-17.6352154588997));
#9264=CARTESIAN_POINT('Ctrl Pts',(-26.295061332806,41.6915321010441,-17.7658797975923));
#9265=CARTESIAN_POINT('Ctrl Pts',(-26.295061332806,41.6915321010441,-17.7658797975923));
#9266=CARTESIAN_POINT('Ctrl Pts',(-26.295061332806,41.3866319916517,-17.8863036523195));
#9267=CARTESIAN_POINT('Ctrl Pts',(-26.3545217120232,41.0538505476253,-17.9994844450059));
#9268=CARTESIAN_POINT('Ctrl Pts',(-26.6094575005743,40.432164168516,-18.1787126925427));
#9269=CARTESIAN_POINT('Ctrl Pts',(-26.8052572776176,40.14362590236,-18.2455693753694));
#9270=CARTESIAN_POINT('Ctrl Pts',(-27.2559905957869,39.697227181252,-18.3358255528225));
#9271=CARTESIAN_POINT('Ctrl Pts',(-27.5353468960521,39.5067960121042,-18.3667437285981));
#9272=CARTESIAN_POINT('Ctrl Pts',(-28.1484345319317,39.2539459288562,-18.4043827853512));
#9273=CARTESIAN_POINT('Ctrl Pts',(-28.4821173645511,39.1915321010441,-18.4119234017692));
#9274=CARTESIAN_POINT('Ctrl Pts',(-29.1080053010609,39.1915321010441,-18.4119234017692));
#9275=CARTESIAN_POINT('Ctrl Pts',(-29.4416881336803,39.2539459288562,-18.4043827853512));
#9276=CARTESIAN_POINT('Ctrl Pts',(-30.0547757695599,39.5067960121042,-18.3667437285981));
#9277=CARTESIAN_POINT('Ctrl Pts',(-30.3341320698251,39.697227181252,-18.3358255528225));
#9278=CARTESIAN_POINT('Ctrl Pts',(-30.7848653879944,40.14362590236,-18.2455693753694));
#9279=CARTESIAN_POINT('Ctrl Pts',(-30.9806651650377,40.432164168516,-18.1787126925427));
#9280=CARTESIAN_POINT('Ctrl Pts',(-31.2356009535887,41.0538505476253,-17.9994844450059));
#9281=CARTESIAN_POINT('Ctrl Pts',(-31.295061332806,41.3866319916517,-17.8863036523195));
#9282=CARTESIAN_POINT('Ctrl Pts',(-31.295061332806,42.0223600026362,-17.6352154588997));
#9283=CARTESIAN_POINT('Ctrl Pts',(-31.2260895128688,42.3675807949546,-17.4776278426165));
#9284=CARTESIAN_POINT('Ctrl Pts',(-30.95523862548,42.9955925725868,-17.1508048084055));
#9285=CARTESIAN_POINT('Ctrl Pts',(-30.7537122028376,43.2788343380328,-16.9821438465083));
#9286=CARTESIAN_POINT('Ctrl Pts',(-30.3077002103262,43.7030327750914,-16.7100751903339));
#9287=CARTESIAN_POINT('Ctrl Pts',(-30.0405259238277,43.8830970093849,-16.5840484145446));
#9288=CARTESIAN_POINT('Ctrl Pts',(-29.4431932108887,44.1275251245074,-16.4064970323244));
#9289=CARTESIAN_POINT('Ctrl Pts',(-29.11233723547,44.1915321010441,-16.3568335820293));
#9290=CARTESIAN_POINT('Ctrl Pts',(-28.795061332806,44.1915321010441,-16.3568335820293));
#9291=CARTESIAN_POINT('',(-26.295061332806,41.6915321010441,-20.));
#9292=CARTESIAN_POINT('',(-26.295061332806,41.6915321010441,20.));
#9293=CARTESIAN_POINT('Origin',(-28.795061332806,41.6915321010441,-20.));
#9294=CARTESIAN_POINT('Origin',(-40.,-30.7011310483684,-19.));
#9295=CARTESIAN_POINT('',(-40.,-30.7011310483684,-19.));
#9296=CARTESIAN_POINT('',(-40.,-31.7011310483684,-20.));
#9297=CARTESIAN_POINT('',(-40.,-5.77584828627628,5.92528276209211));
#9298=CARTESIAN_POINT('',(40.,-30.7011310483684,-19.));
#9299=CARTESIAN_POINT('',(-40.,-30.7011310483684,-19.));
#9300=CARTESIAN_POINT('',(40.,-31.7011310483684,-20.));
#9301=CARTESIAN_POINT('',(40.,-30.7758482862763,-19.0747172379079));
#9302=CARTESIAN_POINT('',(-20.,-31.7011310483684,-20.));
#9303=CARTESIAN_POINT('Origin',(-40.,-11.9332887764186,-19.));
#9304=CARTESIAN_POINT('',(-40.,-11.9332887764186,-19.));
#9305=CARTESIAN_POINT('',(-40.,19.0333556117907,-19.));
#9306=CARTESIAN_POINT('',(40.,-11.9332887764186,-19.));
#9307=CARTESIAN_POINT('',(-40.,-11.9332887764186,-19.));
#9308=CARTESIAN_POINT('',(40.,-30.9666443882093,-19.));
#9309=CARTESIAN_POINT('Origin',(-40.,-10.9332887764186,-20.));
#9310=CARTESIAN_POINT('',(-40.,-10.9332887764186,-20.));
#9311=CARTESIAN_POINT('',(-40.,-0.699966582313925,-30.2333221941047));
#9312=CARTESIAN_POINT('',(40.,-10.9332887764186,-20.));
#9313=CARTESIAN_POINT('',(-20.,-10.9332887764186,-20.));
#9314=CARTESIAN_POINT('',(40.,-25.6999665823139,-5.23332219410464));
#9315=CARTESIAN_POINT('Origin',(-8.88178419700125E-15,8.88178419700125E-15,
-20.));
#9316=CARTESIAN_POINT('',(40.,-47.,-20.));
#9317=CARTESIAN_POINT('',(40.,50.,-20.));
#9318=CARTESIAN_POINT('',(-40.,-47.,-20.));
#9319=CARTESIAN_POINT('',(-20.,-47.,-20.));
#9320=CARTESIAN_POINT('',(-40.,-50.,-20.));
#9321=CARTESIAN_POINT('Origin',(-8.88178419700125E-15,8.88178419700125E-15,
-20.));
#9322=CARTESIAN_POINT('',(-40.,10.9332887764186,-20.));
#9323=CARTESIAN_POINT('',(-40.,-50.,-20.));
#9324=CARTESIAN_POINT('',(40.,10.9332887764186,-20.));
#9325=CARTESIAN_POINT('',(-20.,10.9332887764186,-20.));
#9326=CARTESIAN_POINT('',(40.,50.,-20.));
#9327=CARTESIAN_POINT('Origin',(-40.,50.,0.));
#9328=CARTESIAN_POINT('',(-40.,-50.,-17.));
#9329=CARTESIAN_POINT('',(-40.,-28.5,-38.5));
#9330=CARTESIAN_POINT('',(-40.,-50.,17.));
#9331=CARTESIAN_POINT('',(-40.,-50.,0.));
#9332=CARTESIAN_POINT('',(-40.,-47.,20.));
#9333=CARTESIAN_POINT('',(-40.,-28.5,38.5));
#9334=CARTESIAN_POINT('',(-40.,-31.7011310483684,20.));
#9335=CARTESIAN_POINT('',(-40.,-50.,20.));
#9336=CARTESIAN_POINT('',(-40.,-30.7011310483684,19.));
#9337=CARTESIAN_POINT('',(-40.,-5.77584828627628,-5.92528276209211));
#9338=CARTESIAN_POINT('',(-40.,-11.9332887764186,19.));
#9339=CARTESIAN_POINT('',(-40.,19.0333556117907,19.));
#9340=CARTESIAN_POINT('',(-40.,-10.9332887764186,20.));
#9341=CARTESIAN_POINT('',(-40.,-0.699966582313925,30.2333221941047));
#9342=CARTESIAN_POINT('',(-40.,10.9332887764186,20.));
#9343=CARTESIAN_POINT('',(-40.,-50.,20.));
#9344=CARTESIAN_POINT('',(-40.,11.9332887764186,19.));
#9345=CARTESIAN_POINT('',(-40.,25.6999665823139,5.23332219410463));
#9346=CARTESIAN_POINT('',(-40.,30.7011310483684,19.));
#9347=CARTESIAN_POINT('',(-40.,30.9666443882093,19.));
#9348=CARTESIAN_POINT('',(-40.,31.7011310483684,20.));
#9349=CARTESIAN_POINT('',(-40.,30.7758482862763,19.0747172379079));
#9350=CARTESIAN_POINT('',(-40.,47.,20.));
#9351=CARTESIAN_POINT('',(-40.,-50.,20.));
#9352=CARTESIAN_POINT('',(-40.,50.,17.));
#9353=CARTESIAN_POINT('',(-40.,53.5,13.5));
#9354=CARTESIAN_POINT('',(-40.,50.,-17.));
#9355=CARTESIAN_POINT('',(-40.,50.,0.));
#9356=CARTESIAN_POINT('',(-40.,47.,-20.));
#9357=CARTESIAN_POINT('',(-40.,53.5,-13.5));
#9358=CARTESIAN_POINT('',(-40.,31.7011310483684,-20.));
#9359=CARTESIAN_POINT('',(-40.,-50.,-20.));
#9360=CARTESIAN_POINT('',(-40.,30.7011310483684,-19.));
#9361=CARTESIAN_POINT('',(-40.,30.7758482862763,-19.0747172379079));
#9362=CARTESIAN_POINT('',(-40.,11.9332887764186,-19.));
#9363=CARTESIAN_POINT('',(-40.,30.9666443882093,-19.));
#9364=CARTESIAN_POINT('',(-40.,25.6999665823139,-5.23332219410463));
#9365=CARTESIAN_POINT('',(-40.,48.3343839603864,-7.99999999999999));
#9366=CARTESIAN_POINT('Origin',(-40.,37.8343839603864,-7.99999999999999));
#9367=CARTESIAN_POINT('',(-40.,-48.3343839603864,-7.99999999999999));
#9368=CARTESIAN_POINT('Origin',(-40.,-37.8343839603864,-7.99999999999999));
#9369=CARTESIAN_POINT('',(-40.,-17.5,8.38733349006174E-15));
#9370=CARTESIAN_POINT('Origin',(-40.,1.91963385766348E-15,1.05304653885696E-14));
#9371=CARTESIAN_POINT('Origin',(-40.,30.7011310483684,-19.));
#9372=CARTESIAN_POINT('',(40.,31.7011310483684,-20.));
#9373=CARTESIAN_POINT('',(-20.,31.7011310483684,-20.));
#9374=CARTESIAN_POINT('',(40.,30.7011310483684,-19.));
#9375=CARTESIAN_POINT('',(40.,5.77584828627629,5.9252827620921));
#9376=CARTESIAN_POINT('',(-40.,30.7011310483684,-19.));
#9377=CARTESIAN_POINT('Origin',(-40.,11.9332887764186,-19.));
#9378=CARTESIAN_POINT('',(40.,11.9332887764186,-19.));
#9379=CARTESIAN_POINT('',(40.,-19.0333556117907,-19.));
#9380=CARTESIAN_POINT('',(-40.,11.9332887764186,-19.));
#9381=CARTESIAN_POINT('Origin',(-40.,10.9332887764186,-20.));
#9382=CARTESIAN_POINT('',(40.,0.699966582313925,-30.2333221941046));
#9383=CARTESIAN_POINT('Origin',(40.,-50.,0.));
#9384=CARTESIAN_POINT('',(40.,47.,-20.));
#9385=CARTESIAN_POINT('',(40.,50.,-20.));
#9386=CARTESIAN_POINT('',(40.,50.,-17.));
#9387=CARTESIAN_POINT('',(40.,28.5,-38.5));
#9388=CARTESIAN_POINT('',(40.,50.,17.));
#9389=CARTESIAN_POINT('',(40.,50.,0.));
#9390=CARTESIAN_POINT('',(40.,47.,20.));
#9391=CARTESIAN_POINT('',(40.,28.5,38.5));
#9392=CARTESIAN_POINT('',(40.,31.7011310483684,20.));
#9393=CARTESIAN_POINT('',(40.,50.,20.));
#9394=CARTESIAN_POINT('',(40.,30.7011310483684,19.));
#9395=CARTESIAN_POINT('',(40.,5.77584828627629,-5.9252827620921));
#9396=CARTESIAN_POINT('',(40.,11.9332887764186,19.));
#9397=CARTESIAN_POINT('',(40.,-19.0333556117907,19.));
#9398=CARTESIAN_POINT('',(40.,10.9332887764186,20.));
#9399=CARTESIAN_POINT('',(40.,0.699966582313925,30.2333221941046));
#9400=CARTESIAN_POINT('',(40.,-10.9332887764186,20.));
#9401=CARTESIAN_POINT('',(40.,50.,20.));
#9402=CARTESIAN_POINT('',(40.,-11.9332887764186,19.));
#9403=CARTESIAN_POINT('',(40.,-25.6999665823139,5.23332219410464));
#9404=CARTESIAN_POINT('',(40.,-30.7011310483684,19.));
#9405=CARTESIAN_POINT('',(40.,-30.9666443882093,19.));
#9406=CARTESIAN_POINT('',(40.,-31.7011310483684,20.));
#9407=CARTESIAN_POINT('',(40.,-30.7758482862763,19.0747172379079));
#9408=CARTESIAN_POINT('',(40.,-47.,20.));
#9409=CARTESIAN_POINT('',(40.,50.,20.));
#9410=CARTESIAN_POINT('',(40.,-50.,17.));
#9411=CARTESIAN_POINT('',(40.,-53.5,13.5));
#9412=CARTESIAN_POINT('',(40.,-50.,-17.));
#9413=CARTESIAN_POINT('',(40.,-50.,0.));
#9414=CARTESIAN_POINT('',(40.,-53.5,-13.5));
#9415=CARTESIAN_POINT('',(40.,48.3343839603864,-7.99999999999999));
#9416=CARTESIAN_POINT('Origin',(40.,37.8343839603864,-7.99999999999999));
#9417=CARTESIAN_POINT('',(40.,-48.3343839603864,-7.99999999999999));
#9418=CARTESIAN_POINT('Origin',(40.,-37.8343839603864,-7.99999999999999));
#9419=CARTESIAN_POINT('',(40.,-17.5,8.38733349006174E-15));
#9420=CARTESIAN_POINT('Origin',(40.,1.91963385766348E-15,1.05304653885696E-14));
#9421=CARTESIAN_POINT('Origin',(-8.88178419700125E-15,8.88178419700125E-15,
-20.));
#9422=CARTESIAN_POINT('',(20.,47.,-20.));
#9423=CARTESIAN_POINT('Origin',(-40.,-30.7011310483684,19.));
#9424=CARTESIAN_POINT('',(-20.,-31.7011310483684,20.));
#9425=CARTESIAN_POINT('',(-40.,-30.7011310483684,19.));
#9426=CARTESIAN_POINT('Origin',(-40.,-11.9332887764186,19.));
#9427=CARTESIAN_POINT('',(-40.,-11.9332887764186,19.));
#9428=CARTESIAN_POINT('Origin',(-40.,-10.9332887764186,20.));
#9429=CARTESIAN_POINT('',(-20.,-10.9332887764186,20.));
#9430=CARTESIAN_POINT('Origin',(-8.88178419700125E-15,8.88178419700125E-15,
20.));
#9431=CARTESIAN_POINT('',(-20.,-47.,20.));
#9432=CARTESIAN_POINT('Origin',(-8.88178419700125E-15,8.88178419700125E-15,
20.));
#9433=CARTESIAN_POINT('',(-20.,10.9332887764186,20.));
#9434=CARTESIAN_POINT('Origin',(-40.,30.7011310483684,19.));
#9435=CARTESIAN_POINT('',(-40.,30.7011310483684,19.));
#9436=CARTESIAN_POINT('',(-20.,31.7011310483684,20.));
#9437=CARTESIAN_POINT('Origin',(-40.,11.9332887764186,19.));
#9438=CARTESIAN_POINT('',(-40.,11.9332887764186,19.));
#9439=CARTESIAN_POINT('Origin',(-40.,10.9332887764186,20.));
#9440=CARTESIAN_POINT('Origin',(-8.88178419700125E-15,8.88178419700125E-15,
20.));
#9441=CARTESIAN_POINT('',(20.,47.,20.));
#9442=CARTESIAN_POINT('Origin',(0.,37.8343839603864,-7.99999999999999));
#9443=CARTESIAN_POINT('',(0.,48.3343839603864,-7.99999999999999));
#9444=CARTESIAN_POINT('Origin',(0.,-37.8343839603864,-7.99999999999999));
#9445=CARTESIAN_POINT('',(0.,-48.3343839603864,-7.99999999999999));
#9446=CARTESIAN_POINT('Origin',(0.,1.91963385766348E-15,1.05304653885696E-14));
#9447=CARTESIAN_POINT('',(0.,-17.5,1.26735972870775E-14));
#9448=CARTESIAN_POINT('Origin',(20.,48.5,-18.5));
#9449=CARTESIAN_POINT('',(20.,50.,-17.));
#9450=CARTESIAN_POINT('Origin',(40.,50.,0.));
#9451=CARTESIAN_POINT('',(20.,50.,17.));
#9452=CARTESIAN_POINT('Origin',(20.,48.5,18.5));
#9453=CARTESIAN_POINT('Origin',(-20.,-48.5,-18.5));
#9454=CARTESIAN_POINT('',(-20.,-50.,-17.));
#9455=CARTESIAN_POINT('Origin',(-40.,-50.,0.));
#9456=CARTESIAN_POINT('',(-20.,-50.,17.));
#9457=CARTESIAN_POINT('Origin',(-20.,-48.5,18.5));
#9458=CARTESIAN_POINT('',(16.7192158067658,-37.8343839603864,-8.00000000000001));
#9459=CARTESIAN_POINT('',(-144.,-37.8343839603864,-7.99999999999999));
#9460=CARTESIAN_POINT('',(-140.,-44.0000000000004,8.77546295170416));
#9461=CARTESIAN_POINT('',(0.,0.,0.));
#9462=CARTESIAN_POINT('',(0.,0.,0.));
#9463=CARTESIAN_POINT('',(16.7192158067658,37.8343839603864,-7.99999999999999));
#9464=CARTESIAN_POINT('',(-58.2807841932342,-37.8343839603864,-8.00000000000001));
#9465=CARTESIAN_POINT('',(-58.2807841932342,37.8343839603864,-7.99999999999999));
#9466=CARTESIAN_POINT('',(-144.,37.8343839603864,-8.00000000000004));
#9467=CARTESIAN_POINT('',(144.,-37.8343839603864,-8.00000000000001));
#9468=CARTESIAN_POINT('',(144.,37.8343839603864,-8.00000000000001));
#9469=CARTESIAN_POINT('',(0.,0.,0.));
#9470=CARTESIAN_POINT('',(0.,0.,0.));
#9471=CARTESIAN_POINT('',(0.,0.,0.));
#9472=CARTESIAN_POINT('',(-55.2807841932342,5.43594652054891E-15,5.38458166943201E-16));
#9473=CARTESIAN_POINT('',(13.7192158067658,7.17920352259705E-15,5.38458166943178E-16));
#9474=CARTESIAN_POINT('',(-20.7807841932342,3.4764508291665E-15,-9.99200722162641E-15));
#9475=UNCERTAINTY_MEASURE_WITH_UNIT(LENGTH_MEASURE(0.01),#9497,
'DISTANCE_ACCURACY_VALUE',
'Maximum model space distance between geometric entities at asserted c
onnectivities');
#9476=UNCERTAINTY_MEASURE_WITH_UNIT(LENGTH_MEASURE(0.01),#9497,
'DISTANCE_ACCURACY_VALUE',
'Maximum model space distance between geometric entities at asserted c
onnectivities');
#9477=UNCERTAINTY_MEASURE_WITH_UNIT(LENGTH_MEASURE(0.01),#9497,
'DISTANCE_ACCURACY_VALUE',
'Maximum model space distance between geometric entities at asserted c
onnectivities');
#9478=UNCERTAINTY_MEASURE_WITH_UNIT(LENGTH_MEASURE(0.01),#9497,
'DISTANCE_ACCURACY_VALUE',
'Maximum model space distance between geometric entities at asserted c
onnectivities');
#9479=UNCERTAINTY_MEASURE_WITH_UNIT(LENGTH_MEASURE(0.01),#9497,
'DISTANCE_ACCURACY_VALUE',
'Maximum model space distance between geometric entities at asserted c
onnectivities');
#9480=UNCERTAINTY_MEASURE_WITH_UNIT(LENGTH_MEASURE(0.01),#9497,
'DISTANCE_ACCURACY_VALUE',
'Maximum model space distance between geometric entities at asserted c
onnectivities');
#9481=UNCERTAINTY_MEASURE_WITH_UNIT(LENGTH_MEASURE(0.01),#9497,
'DISTANCE_ACCURACY_VALUE',
'Maximum model space distance between geometric entities at asserted c
onnectivities');
#9482=UNCERTAINTY_MEASURE_WITH_UNIT(LENGTH_MEASURE(0.01),#9497,
'DISTANCE_ACCURACY_VALUE',
'Maximum model space distance between geometric entities at asserted c
onnectivities');
#9483=UNCERTAINTY_MEASURE_WITH_UNIT(LENGTH_MEASURE(0.01),#9497,
'DISTANCE_ACCURACY_VALUE',
'Maximum model space distance between geometric entities at asserted c
onnectivities');
#9484=UNCERTAINTY_MEASURE_WITH_UNIT(LENGTH_MEASURE(0.01),#9497,
'DISTANCE_ACCURACY_VALUE',
'Maximum model space distance between geometric entities at asserted c
onnectivities');
#9485=UNCERTAINTY_MEASURE_WITH_UNIT(LENGTH_MEASURE(0.01),#9497,
'DISTANCE_ACCURACY_VALUE',
'Maximum model space distance between geometric entities at asserted c
onnectivities');
#9486=(
GEOMETRIC_REPRESENTATION_CONTEXT(3)
GLOBAL_UNCERTAINTY_ASSIGNED_CONTEXT((#9475))
GLOBAL_UNIT_ASSIGNED_CONTEXT((#9497,#9499,#9500))
REPRESENTATION_CONTEXT('','3D')
);
#9487=(
GEOMETRIC_REPRESENTATION_CONTEXT(3)
GLOBAL_UNCERTAINTY_ASSIGNED_CONTEXT((#9476))
GLOBAL_UNIT_ASSIGNED_CONTEXT((#9497,#9499,#9500))
REPRESENTATION_CONTEXT('','3D')
);
#9488=(
GEOMETRIC_REPRESENTATION_CONTEXT(3)
GLOBAL_UNCERTAINTY_ASSIGNED_CONTEXT((#9477))
GLOBAL_UNIT_ASSIGNED_CONTEXT((#9497,#9499,#9500))
REPRESENTATION_CONTEXT('','3D')
);
#9489=(
GEOMETRIC_REPRESENTATION_CONTEXT(3)
GLOBAL_UNCERTAINTY_ASSIGNED_CONTEXT((#9478))
GLOBAL_UNIT_ASSIGNED_CONTEXT((#9497,#9499,#9500))
REPRESENTATION_CONTEXT('','3D')
);
#9490=(
GEOMETRIC_REPRESENTATION_CONTEXT(3)
GLOBAL_UNCERTAINTY_ASSIGNED_CONTEXT((#9479))
GLOBAL_UNIT_ASSIGNED_CONTEXT((#9497,#9499,#9500))
REPRESENTATION_CONTEXT('','3D')
);
#9491=(
GEOMETRIC_REPRESENTATION_CONTEXT(3)
GLOBAL_UNCERTAINTY_ASSIGNED_CONTEXT((#9480))
GLOBAL_UNIT_ASSIGNED_CONTEXT((#9497,#9499,#9500))
REPRESENTATION_CONTEXT('','3D')
);
#9492=(
GEOMETRIC_REPRESENTATION_CONTEXT(3)
GLOBAL_UNCERTAINTY_ASSIGNED_CONTEXT((#9481))
GLOBAL_UNIT_ASSIGNED_CONTEXT((#9497,#9499,#9500))
REPRESENTATION_CONTEXT('','3D')
);
#9493=(
GEOMETRIC_REPRESENTATION_CONTEXT(3)
GLOBAL_UNCERTAINTY_ASSIGNED_CONTEXT((#9482))
GLOBAL_UNIT_ASSIGNED_CONTEXT((#9497,#9499,#9500))
REPRESENTATION_CONTEXT('','3D')
);
#9494=(
GEOMETRIC_REPRESENTATION_CONTEXT(3)
GLOBAL_UNCERTAINTY_ASSIGNED_CONTEXT((#9483))
GLOBAL_UNIT_ASSIGNED_CONTEXT((#9497,#9499,#9500))
REPRESENTATION_CONTEXT('','3D')
);
#9495=(
GEOMETRIC_REPRESENTATION_CONTEXT(3)
GLOBAL_UNCERTAINTY_ASSIGNED_CONTEXT((#9484))
GLOBAL_UNIT_ASSIGNED_CONTEXT((#9497,#9499,#9500))
REPRESENTATION_CONTEXT('','3D')
);
#9496=(
GEOMETRIC_REPRESENTATION_CONTEXT(3)
GLOBAL_UNCERTAINTY_ASSIGNED_CONTEXT((#9485))
GLOBAL_UNIT_ASSIGNED_CONTEXT((#9497,#9499,#9500))
REPRESENTATION_CONTEXT('','3D')
);
#9497=(
LENGTH_UNIT()
NAMED_UNIT(*)
SI_UNIT(.MILLI.,.METRE.)
);
#9498=(
LENGTH_UNIT()
NAMED_UNIT(*)
SI_UNIT($,.METRE.)
);
#9499=(
NAMED_UNIT(*)
PLANE_ANGLE_UNIT()
SI_UNIT($,.RADIAN.)
);
#9500=(
NAMED_UNIT(*)
SI_UNIT($,.STERADIAN.)
SOLID_ANGLE_UNIT()
);
#9501=SHAPE_DEFINITION_REPRESENTATION(#9511,#9538);
#9502=SHAPE_DEFINITION_REPRESENTATION(#9512,#9539);
#9503=SHAPE_DEFINITION_REPRESENTATION(#9513,#9540);
#9504=SHAPE_DEFINITION_REPRESENTATION(#9514,#9541);
#9505=SHAPE_DEFINITION_REPRESENTATION(#9515,#9542);
#9506=SHAPE_DEFINITION_REPRESENTATION(#9516,#9543);
#9507=SHAPE_DEFINITION_REPRESENTATION(#9517,#9544);
#9508=SHAPE_DEFINITION_REPRESENTATION(#9518,#9545);
#9509=SHAPE_DEFINITION_REPRESENTATION(#9519,#9546);
#9510=SHAPE_DEFINITION_REPRESENTATION(#9520,#9547);
#9511=PRODUCT_DEFINITION_SHAPE('',$,#9549);
#9512=PRODUCT_DEFINITION_SHAPE('',$,#9550);
#9513=PRODUCT_DEFINITION_SHAPE('',$,#9551);
#9514=PRODUCT_DEFINITION_SHAPE('',$,#9552);
#9515=PRODUCT_DEFINITION_SHAPE('',$,#9553);
#9516=PRODUCT_DEFINITION_SHAPE('',$,#9554);
#9517=PRODUCT_DEFINITION_SHAPE('',$,#9555);
#9518=PRODUCT_DEFINITION_SHAPE('',$,#9556);
#9519=PRODUCT_DEFINITION_SHAPE('',$,#9557);
#9520=PRODUCT_DEFINITION_SHAPE('',$,#9558);
#9521=PRODUCT_DEFINITION_SHAPE($,$,#62);
#9522=PRODUCT_DEFINITION_SHAPE($,$,#63);
#9523=PRODUCT_DEFINITION_SHAPE($,$,#64);
#9524=PRODUCT_DEFINITION_SHAPE($,$,#65);
#9525=PRODUCT_DEFINITION_SHAPE($,$,#66);
#9526=PRODUCT_DEFINITION_SHAPE($,$,#67);
#9527=PRODUCT_DEFINITION_SHAPE($,$,#68);
#9528=PRODUCT_DEFINITION_SHAPE($,$,#69);
#9529=PRODUCT_DEFINITION_SHAPE($,$,#70);
#9530=PRODUCT_DEFINITION_SHAPE($,$,#71);
#9531=PRODUCT_DEFINITION_SHAPE($,$,#72);
#9532=PRODUCT_DEFINITION_SHAPE($,$,#73);
#9533=PRODUCT_DEFINITION_SHAPE($,$,#74);
#9534=PRODUCT_DEFINITION_SHAPE($,$,#75);
#9535=PRODUCT_DEFINITION_SHAPE($,$,#76);
#9536=PRODUCT_DEFINITION_SHAPE($,$,#77);
#9537=PRODUCT_DEFINITION_SHAPE($,$,#78);
#9538=SHAPE_REPRESENTATION('',(#5122,#5809,#5810,#5811,#5812,#5813,#5814,
#5815,#5816,#5817,#5818,#5819,#5820,#5821,#5822,#5823,#5824,#5825),#9486);
#9539=SHAPE_REPRESENTATION('',(#5123),#9487);
#9540=SHAPE_REPRESENTATION('',(#5213),#9488);
#9541=SHAPE_REPRESENTATION('',(#5298),#9489);
#9542=SHAPE_REPRESENTATION('',(#5515),#9490);
#9543=SHAPE_REPRESENTATION('',(#5542),#9491);
#9544=SHAPE_REPRESENTATION('',(#5556),#9492);
#9545=SHAPE_REPRESENTATION('',(#5562),#9493);
#9546=SHAPE_REPRESENTATION('',(#5576),#9494);
#9547=SHAPE_REPRESENTATION('',(#5757),#9495);
#9548=PRODUCT_DEFINITION_CONTEXT('part definition',#9580,'design');
#9549=PRODUCT_DEFINITION('MAS-267','MAS-267',#9559,#9548);
#9550=PRODUCT_DEFINITION('End_plates_02','End_plates_02',#9560,#9548);
#9551=PRODUCT_DEFINITION('End_plates','End_plates',#9561,#9548);
#9552=PRODUCT_DEFINITION('Ball Bearing - Small','Ball Bearing - Small',
#9562,#9548);
#9553=PRODUCT_DEFINITION(
'Broached Hexagon Socket Head Cap Screw ASME B18.3.1M - M6x1 x 16 Stee
l Grade 2 Plain v1',
'Broached Hexagon Socket Head Cap Screw ASME B18.3.1M - M6x1 x 16 Stee
l Grade 2 Plain v1',#9563,#9548);
#9554=PRODUCT_DEFINITION('Guide_Shaft_02','Guide_Shaft_02',#9564,#9548);
#9555=PRODUCT_DEFINITION('Cylinder_Tube','Cylinder_Tube',#9565,#9548);
#9556=PRODUCT_DEFINITION('Guide_Shaft','Guide_Shaft',#9566,#9548);
#9557=PRODUCT_DEFINITION('Ball Bearing - Large','Ball Bearing - Large',
#9567,#9548);
#9558=PRODUCT_DEFINITION('Slide_Block','Slide_Block',#9568,#9548);
#9559=PRODUCT_DEFINITION_FORMATION('',$,#9582);
#9560=PRODUCT_DEFINITION_FORMATION('',$,#9583);
#9561=PRODUCT_DEFINITION_FORMATION('',$,#9584);
#9562=PRODUCT_DEFINITION_FORMATION('',$,#9585);
#9563=PRODUCT_DEFINITION_FORMATION('',$,#9586);
#9564=PRODUCT_DEFINITION_FORMATION('',$,#9587);
#9565=PRODUCT_DEFINITION_FORMATION('',$,#9588);
#9566=PRODUCT_DEFINITION_FORMATION('',$,#9589);
#9567=PRODUCT_DEFINITION_FORMATION('',$,#9590);
#9568=PRODUCT_DEFINITION_FORMATION('',$,#9591);
#9569=PRODUCT_RELATED_PRODUCT_CATEGORY('MAS-267','MAS-267',(#9582));
#9570=PRODUCT_RELATED_PRODUCT_CATEGORY('End_plates_02','End_plates_02',
(#9583));
#9571=PRODUCT_RELATED_PRODUCT_CATEGORY('End_plates','End_plates',(#9584));
#9572=PRODUCT_RELATED_PRODUCT_CATEGORY('Ball Bearing - Small',
'Ball Bearing - Small',(#9585));
#9573=PRODUCT_RELATED_PRODUCT_CATEGORY(
'Broached Hexagon Socket Head Cap Screw ASME B18.3.1M - M6x1 x 16 Stee
l Grade 2 Plain v1',
'Broached Hexagon Socket Head Cap Screw ASME B18.3.1M - M6x1 x 16 Stee
l Grade 2 Plain v1',(#9586));
#9574=PRODUCT_RELATED_PRODUCT_CATEGORY('Guide_Shaft_02',
'Guide_Shaft_02',(#9587));
#9575=PRODUCT_RELATED_PRODUCT_CATEGORY('Cylinder_Tube','Cylinder_Tube',
(#9588));
#9576=PRODUCT_RELATED_PRODUCT_CATEGORY('Guide_Shaft','Guide_Shaft',(#9589));
#9577=PRODUCT_RELATED_PRODUCT_CATEGORY('Ball Bearing - Large',
'Ball Bearing - Large',(#9590));
#9578=PRODUCT_RELATED_PRODUCT_CATEGORY('Slide_Block','Slide_Block',(#9591));
#9579=APPLICATION_PROTOCOL_DEFINITION('international standard',
'automotive_design',2009,#9580);
#9580=APPLICATION_CONTEXT(
'Core Data for Automotive Mechanical Design Process');
#9581=PRODUCT_CONTEXT('part definition',#9580,'mechanical');
#9582=PRODUCT('MAS-267','MAS-267',$,(#9581));
#9583=PRODUCT('End_plates_02','End_plates_02',$,(#9581));
#9584=PRODUCT('End_plates','End_plates',$,(#9581));
#9585=PRODUCT('Ball Bearing - Small','Ball Bearing - Small',$,(#9581));
#9586=PRODUCT(
'Broached Hexagon Socket Head Cap Screw ASME B18.3.1M - M6x1 x 16 Stee
l Grade 2 Plain v1',
'Broached Hexagon Socket Head Cap Screw ASME B18.3.1M - M6x1 x 16 Stee
l Grade 2 Plain v1',
'Broached Hexagon Socket Head Cap Screw ASME B18.3.1M - M6x1 x 16',(#9581));
#9587=PRODUCT('Guide_Shaft_02','Guide_Shaft_02',$,(#9581));
#9588=PRODUCT('Cylinder_Tube','Cylinder_Tube',$,(#9581));
#9589=PRODUCT('Guide_Shaft','Guide_Shaft',$,(#9581));
#9590=PRODUCT('Ball Bearing - Large','Ball Bearing - Large',$,(#9581));
#9591=PRODUCT('Slide_Block','Slide_Block',$,(#9581));
#9592=PRESENTATION_STYLE_ASSIGNMENT((#9595));
#9593=PRESENTATION_STYLE_ASSIGNMENT((#9596));
#9594=PRESENTATION_STYLE_ASSIGNMENT((#9597));
#9595=SURFACE_STYLE_USAGE(.BOTH.,#9598);
#9596=SURFACE_STYLE_USAGE(.BOTH.,#9599);
#9597=SURFACE_STYLE_USAGE(.BOTH.,#9600);
#9598=SURFACE_SIDE_STYLE('',(#9601));
#9599=SURFACE_SIDE_STYLE('',(#9602));
#9600=SURFACE_SIDE_STYLE('',(#9603));
#9601=SURFACE_STYLE_FILL_AREA(#9604);
#9602=SURFACE_STYLE_FILL_AREA(#9605);
#9603=SURFACE_STYLE_FILL_AREA(#9606);
#9604=FILL_AREA_STYLE('Steel - Satin',(#9607));
#9605=FILL_AREA_STYLE('Opaque(245,245,246)',(#9608));
#9606=FILL_AREA_STYLE('Opaque(160,160,160)',(#9609));
#9607=FILL_AREA_STYLE_COLOUR('Steel - Satin',#9610);
#9608=FILL_AREA_STYLE_COLOUR('Opaque(245,245,246)',#9611);
#9609=FILL_AREA_STYLE_COLOUR('Opaque(160,160,160)',#9612);
#9610=COLOUR_RGB('Steel - Satin', 0.66274510, 0.83137255, 0.94901961);
#9611=COLOUR_RGB('Opaque(245,245,246)', 0.66274510, 0.83137255, 0.94901961);
#9612=COLOUR_RGB('Opaque(160,160,160)', 0.40784314, 0.44705882, 0.49803922);
ENDSEC;
END-ISO-10303-21;
